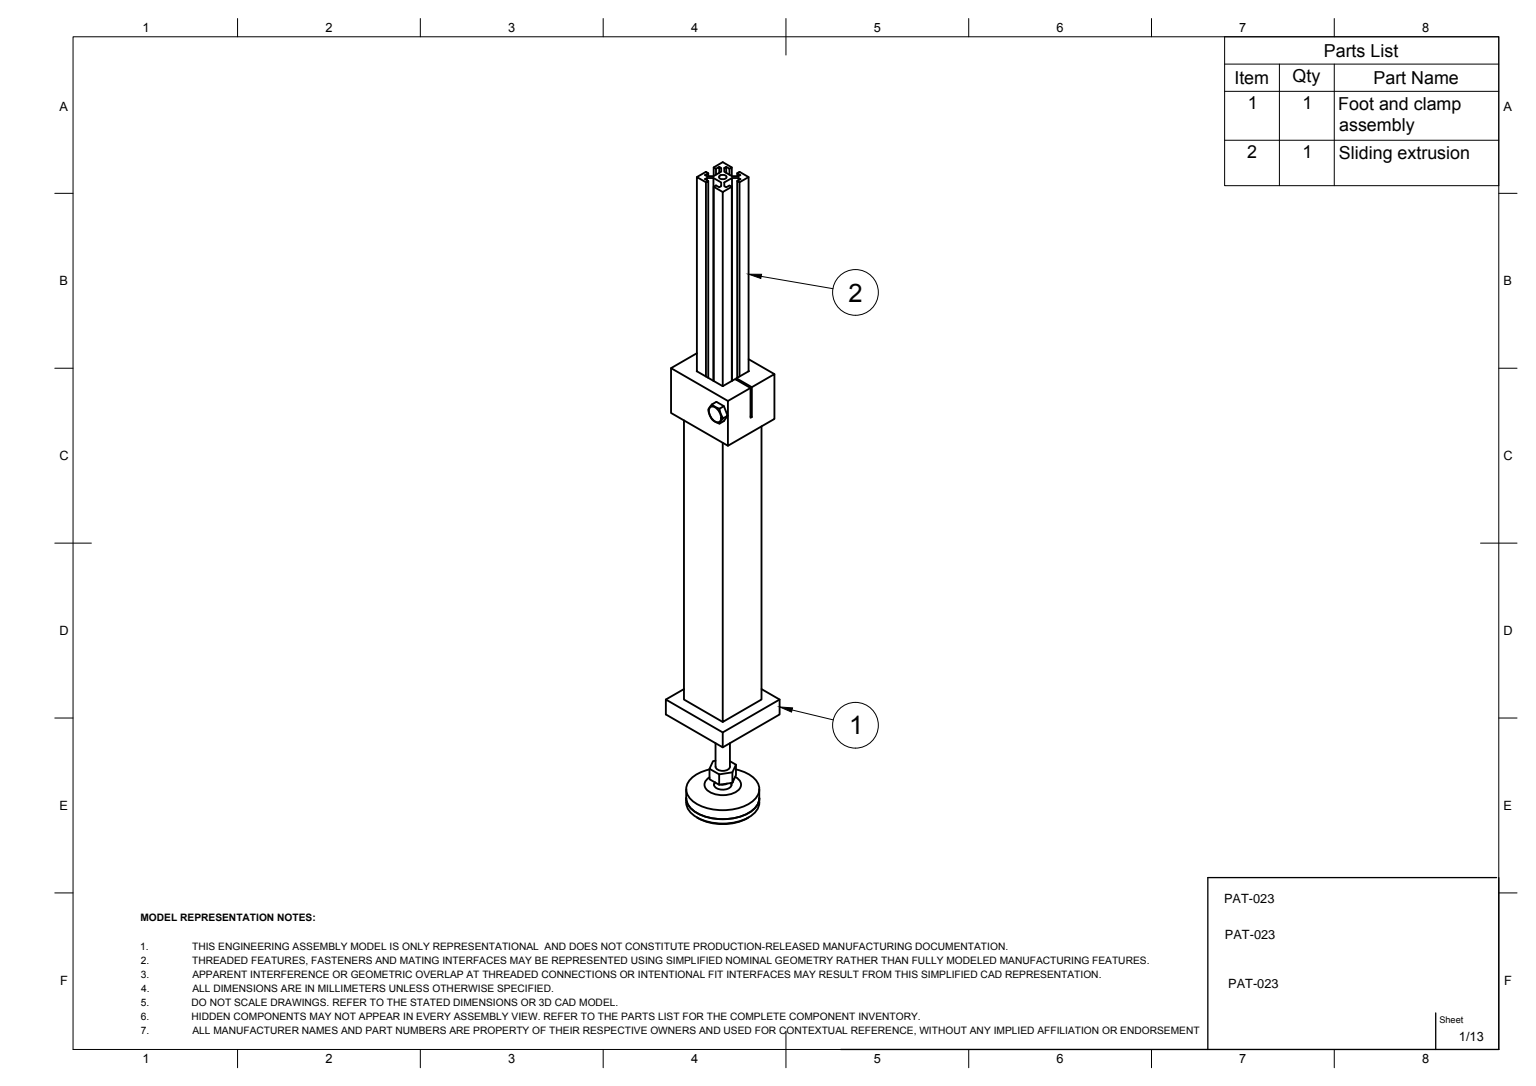
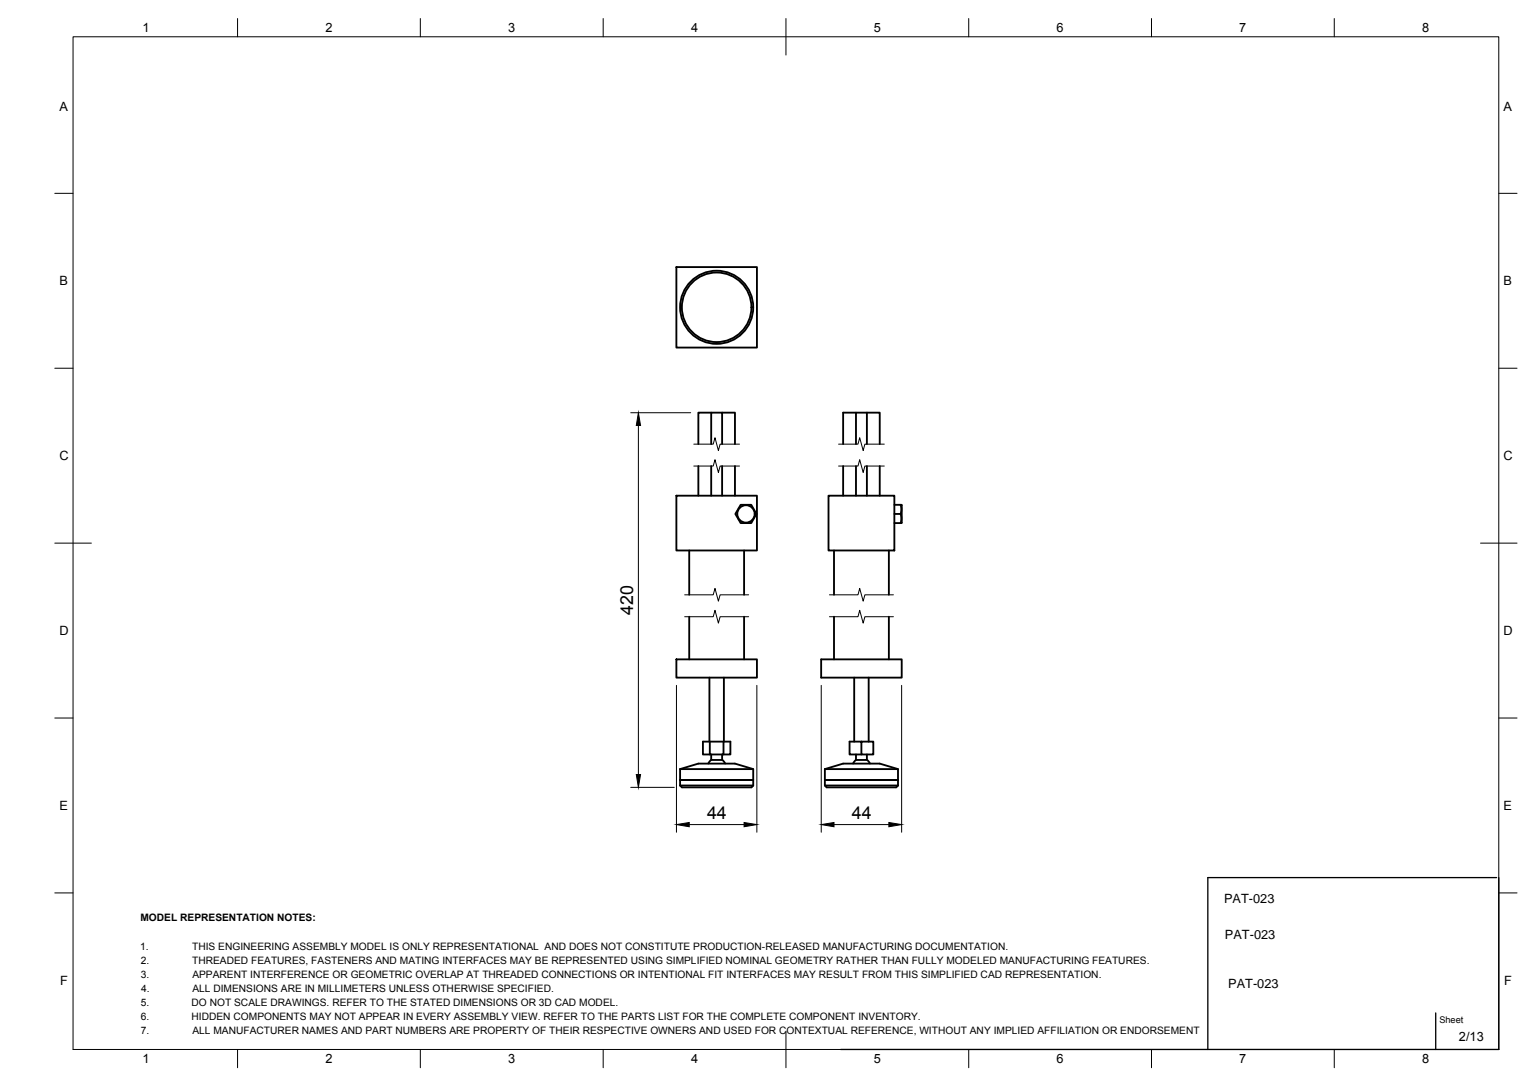
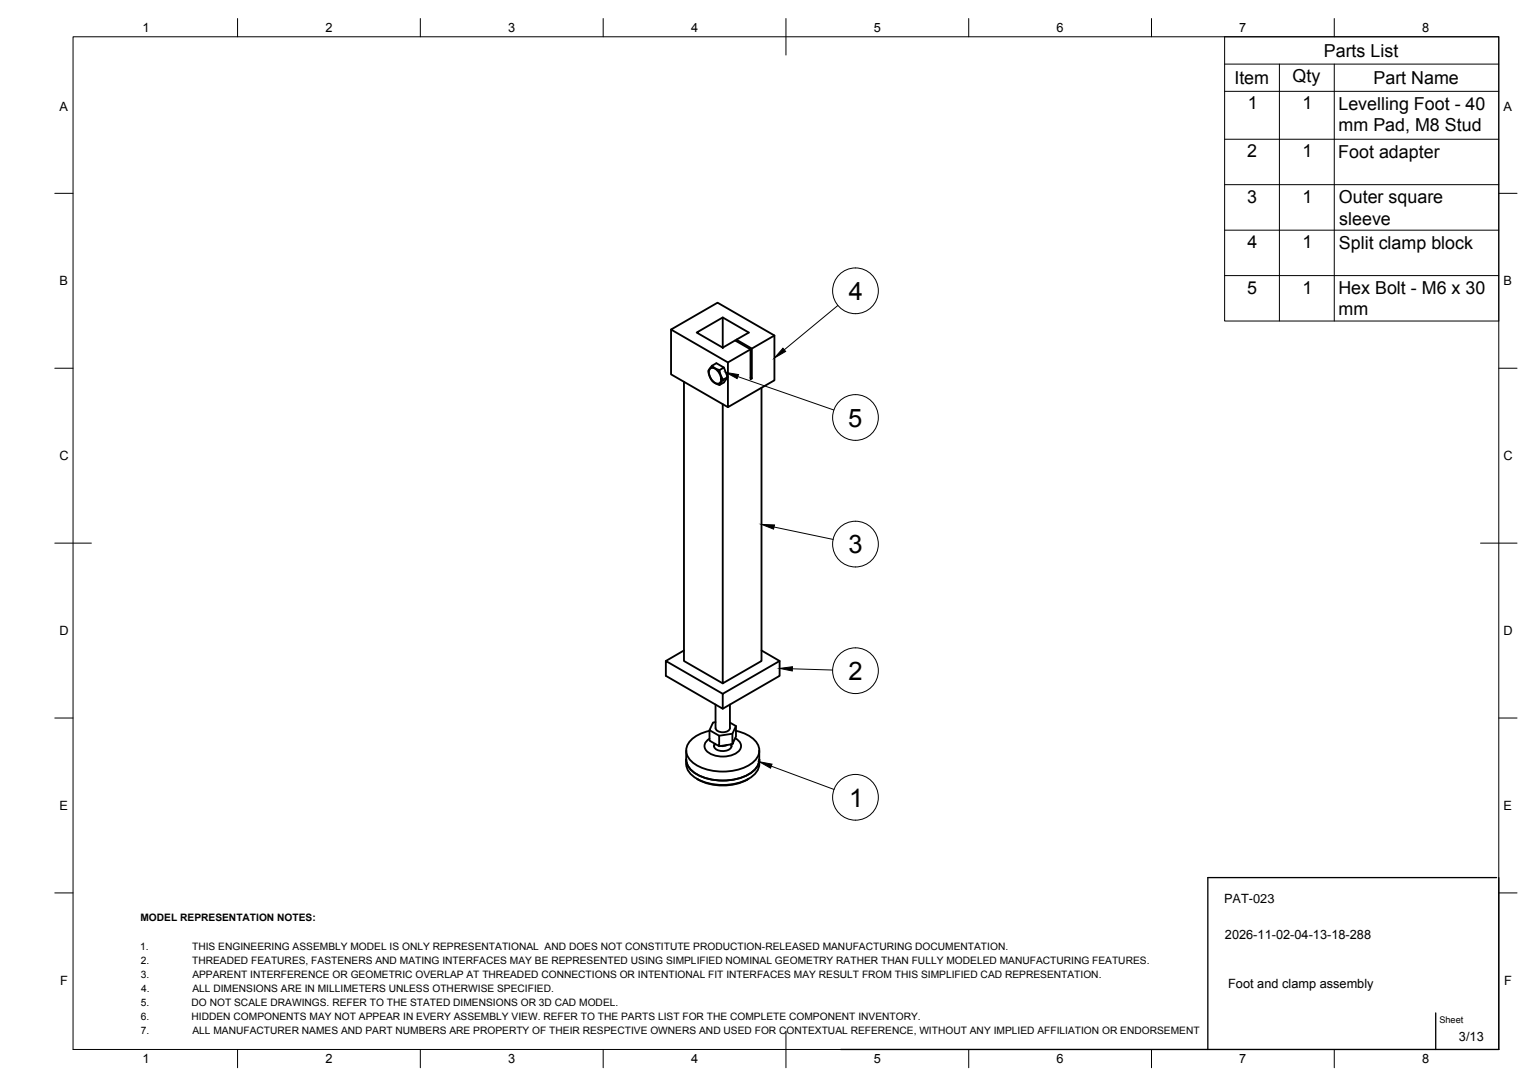
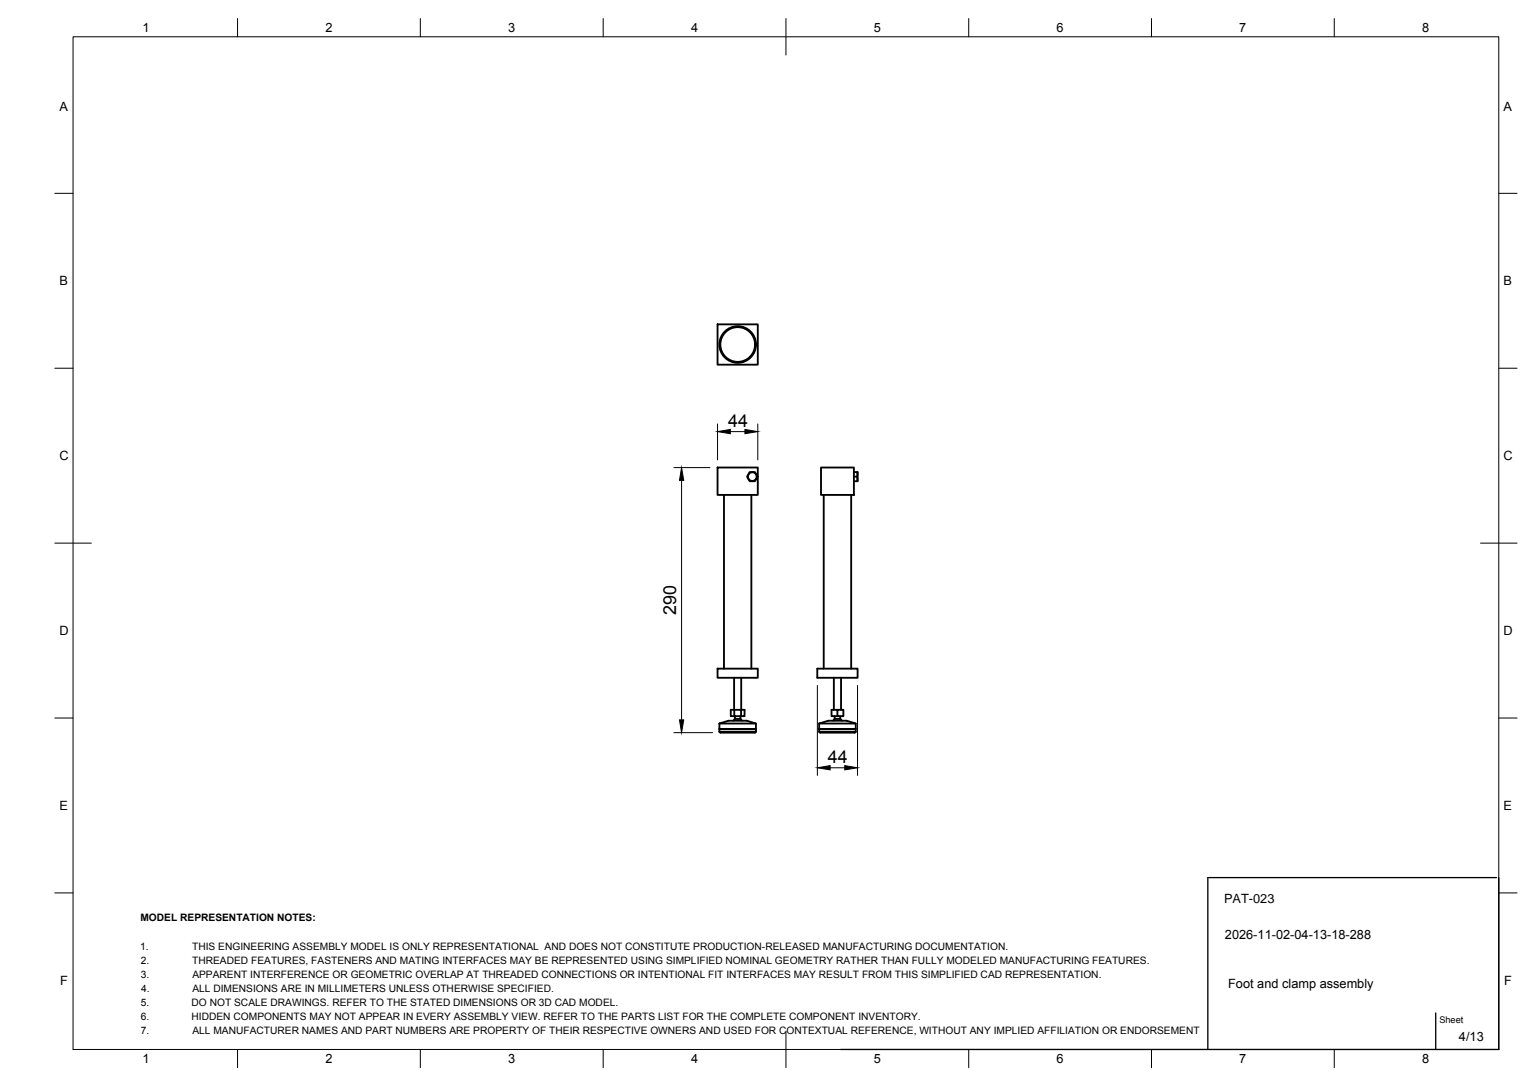
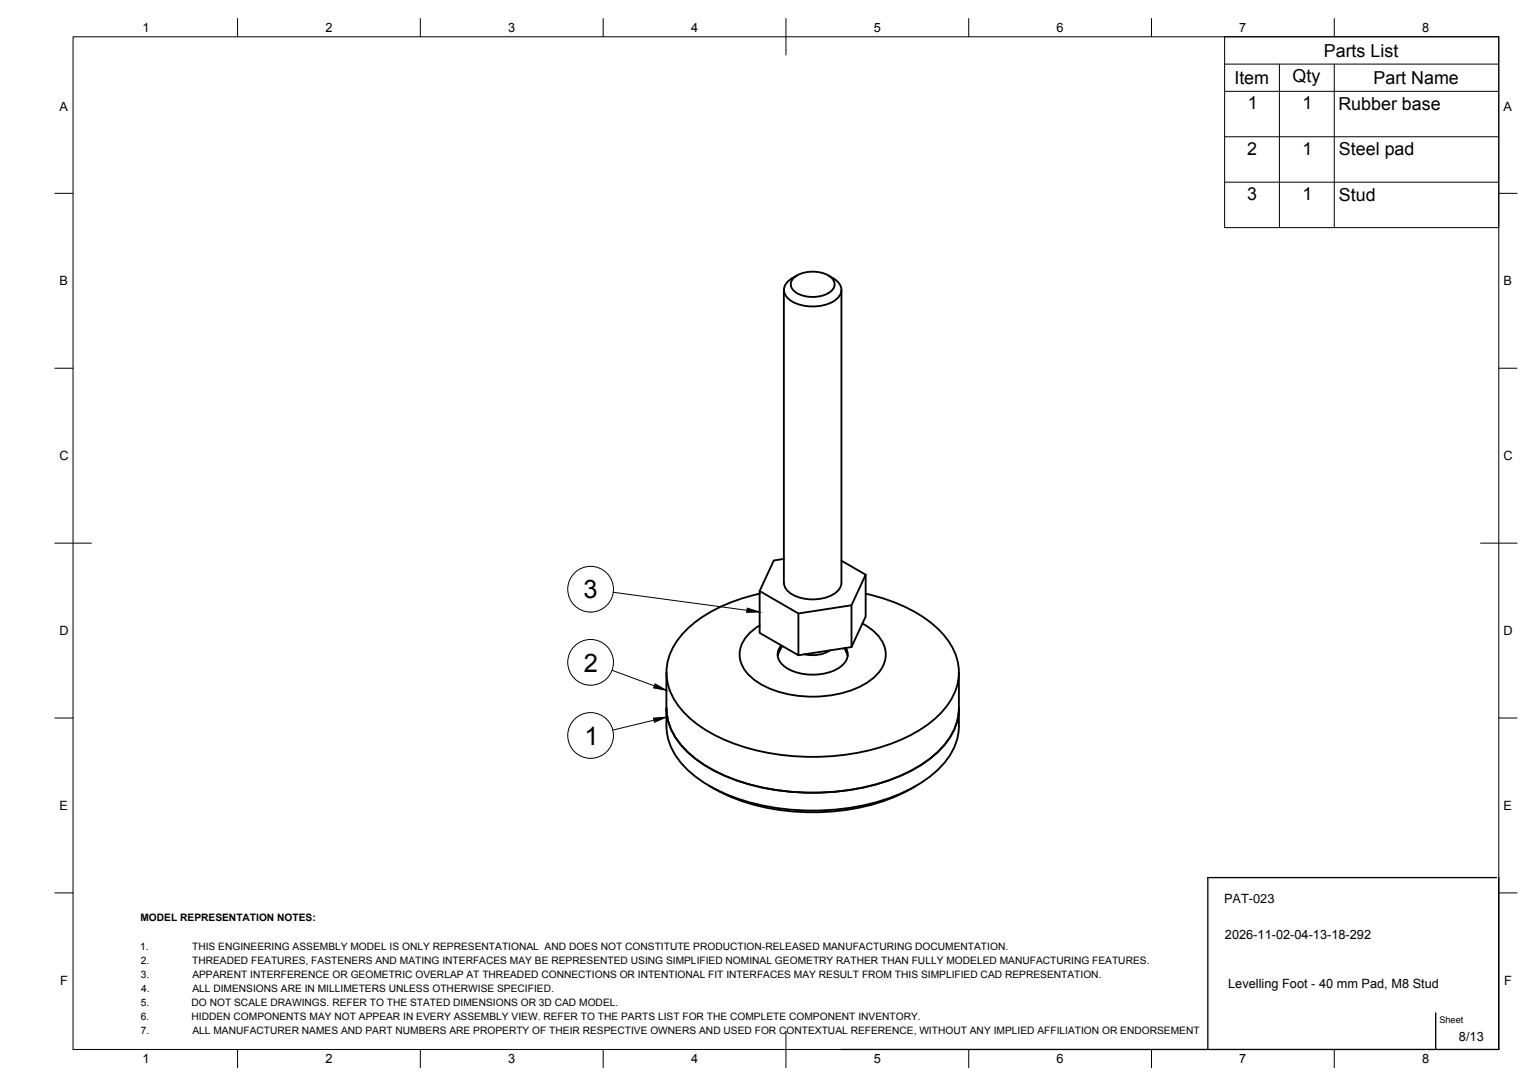
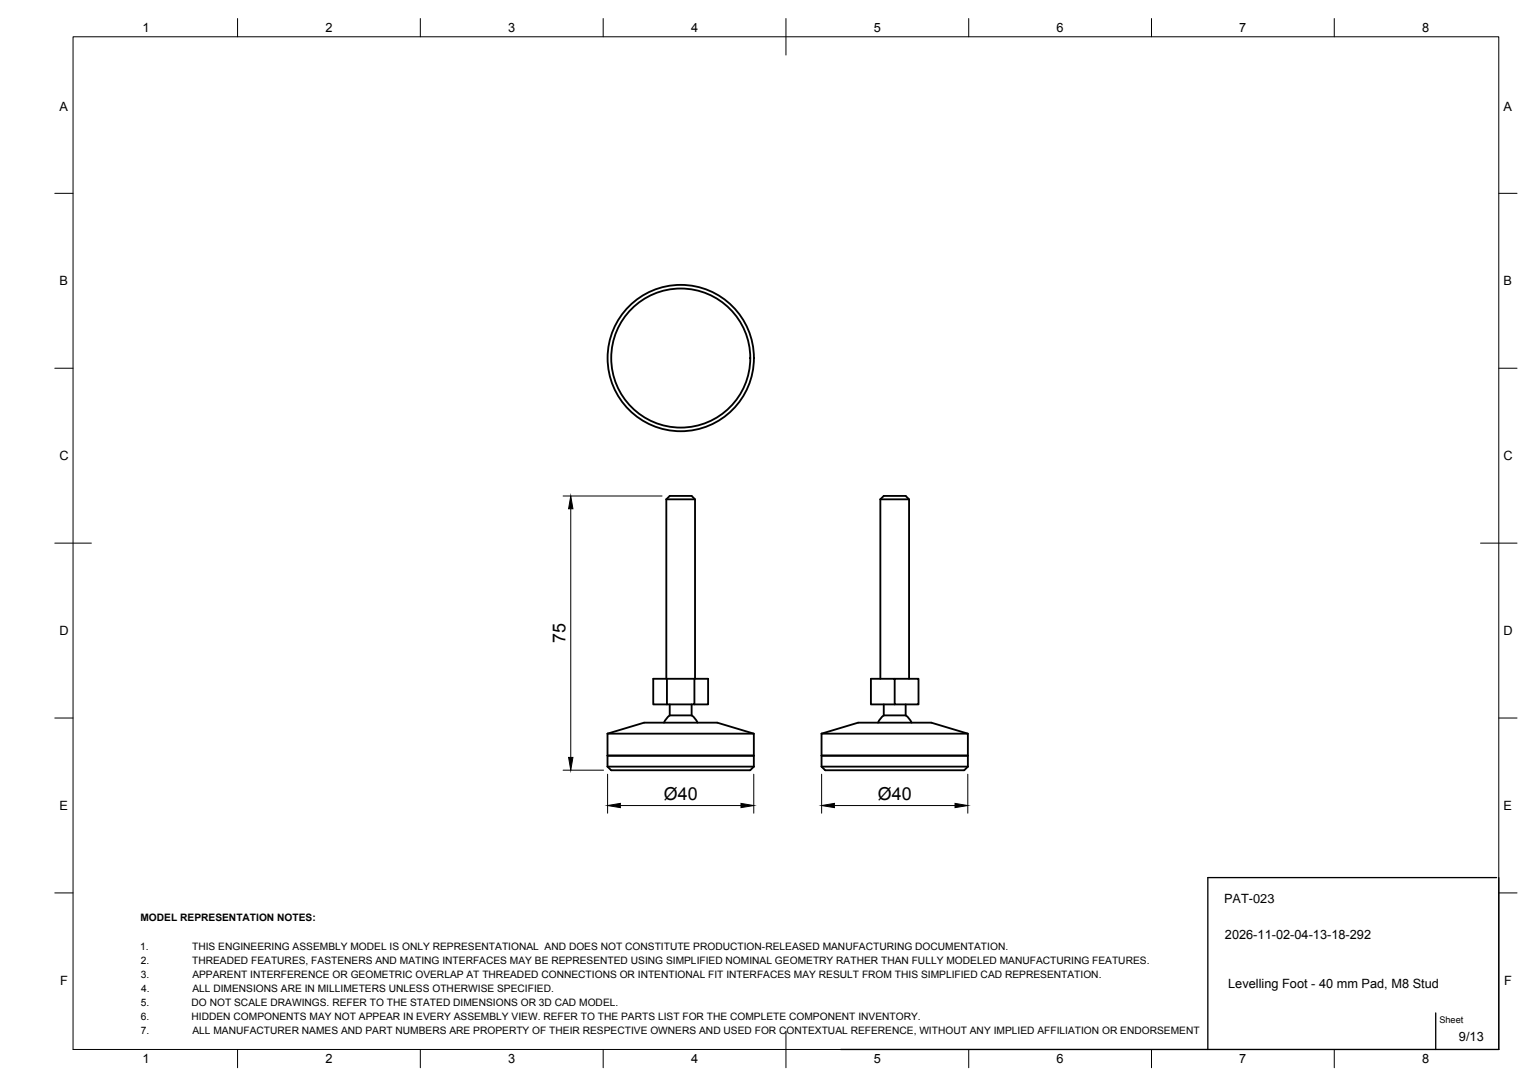
ISO-10303-21;
HEADER;
/* Generated by software containing ST-Developer
 * from STEP Tools, Inc. (www.steptools.com) 
 */

FILE_DESCRIPTION(
/* description */ ('PAT-023'),
/* implementation_level */ '2;1');

FILE_NAME(
/* name */ 'PAT-023',
/* time_stamp */ '2026-10-29T15:47:46-07:00',
/* author */ (''),
/* organization */ (''),
/* preprocessor_version */ 'ST-DEVELOPER v20.2',
/* originating_system */ 'Autodesk Translation Framework v15.17.0.0',
/* authorisation */ '');

FILE_SCHEMA (('AUTOMOTIVE_DESIGN { 1 0 10303 214 3 1 1 }'));
ENDSEC;

DATA;
#10=MECHANICAL_DESIGN_GEOMETRIC_PRESENTATION_REPRESENTATION('',(#84,#85,
#86,#87,#88,#89,#90,#91),#3773);
#11=(
BOUNDED_CURVE()
B_SPLINE_CURVE(2,(#3418,#3419,#3420),.UNSPECIFIED.,.F.,.F.)
B_SPLINE_CURVE_WITH_KNOTS((3,3),(0.144988513094728,0.791574906712449),
 .UNSPECIFIED.)
CURVE()
GEOMETRIC_REPRESENTATION_ITEM()
RATIONAL_B_SPLINE_CURVE((1.09282032302755,1.26188021535082,1.09282032302931))
REPRESENTATION_ITEM('')
);
#12=(
BOUNDED_CURVE()
B_SPLINE_CURVE(2,(#3422,#3423,#3424),.UNSPECIFIED.,.F.,.F.)
B_SPLINE_CURVE_WITH_KNOTS((3,3),(0.144988513094728,0.791574906712449),
 .UNSPECIFIED.)
CURVE()
GEOMETRIC_REPRESENTATION_ITEM()
RATIONAL_B_SPLINE_CURVE((1.09282032302755,1.26188021535082,1.09282032302931))
REPRESENTATION_ITEM('')
);
#13=(
BOUNDED_CURVE()
B_SPLINE_CURVE(2,(#3426,#3427,#3428),.UNSPECIFIED.,.F.,.F.)
B_SPLINE_CURVE_WITH_KNOTS((3,3),(0.144988513094728,0.791574906712449),
 .UNSPECIFIED.)
CURVE()
GEOMETRIC_REPRESENTATION_ITEM()
RATIONAL_B_SPLINE_CURVE((1.09282032302755,1.26188021535082,1.09282032302931))
REPRESENTATION_ITEM('')
);
#14=(
BOUNDED_CURVE()
B_SPLINE_CURVE(2,(#3430,#3431,#3432),.UNSPECIFIED.,.F.,.F.)
B_SPLINE_CURVE_WITH_KNOTS((3,3),(0.144988513094728,0.791574906712449),
 .UNSPECIFIED.)
CURVE()
GEOMETRIC_REPRESENTATION_ITEM()
RATIONAL_B_SPLINE_CURVE((1.09282032302755,1.26188021535082,1.09282032302931))
REPRESENTATION_ITEM('')
);
#15=(
BOUNDED_CURVE()
B_SPLINE_CURVE(2,(#3434,#3435,#3436),.UNSPECIFIED.,.F.,.F.)
B_SPLINE_CURVE_WITH_KNOTS((3,3),(0.144988513094728,0.791574906712449),
 .UNSPECIFIED.)
CURVE()
GEOMETRIC_REPRESENTATION_ITEM()
RATIONAL_B_SPLINE_CURVE((1.09282032302755,1.26188021535082,1.09282032302931))
REPRESENTATION_ITEM('')
);
#16=(
BOUNDED_CURVE()
B_SPLINE_CURVE(2,(#3437,#3438,#3439),.UNSPECIFIED.,.F.,.F.)
B_SPLINE_CURVE_WITH_KNOTS((3,3),(0.144988513094727,0.791574906712449),
 .UNSPECIFIED.)
CURVE()
GEOMETRIC_REPRESENTATION_ITEM()
RATIONAL_B_SPLINE_CURVE((1.09282032302755,1.26188021535082,1.09282032302931))
REPRESENTATION_ITEM('')
);
#17=ITEM_DEFINED_TRANSFORMATION($,$,#2384,#2423);
#18=ITEM_DEFINED_TRANSFORMATION($,$,#2392,#2424);
#19=ITEM_DEFINED_TRANSFORMATION($,$,#2403,#2425);
#20=ITEM_DEFINED_TRANSFORMATION($,$,#2336,#2443);
#21=ITEM_DEFINED_TRANSFORMATION($,$,#2346,#2444);
#22=ITEM_DEFINED_TRANSFORMATION($,$,#2357,#2445);
#23=ITEM_DEFINED_TRANSFORMATION($,$,#2383,#2446);
#24=ITEM_DEFINED_TRANSFORMATION($,$,#2426,#2447);
#25=ITEM_DEFINED_TRANSFORMATION($,$,#2449,#2499);
#26=ITEM_DEFINED_TRANSFORMATION($,$,#2335,#2500);
#27=ITEM_DEFINED_TRANSFORMATION($,$,#2448,#2501);
#28=(
REPRESENTATION_RELATIONSHIP($,$,#3819,#3818)
REPRESENTATION_RELATIONSHIP_WITH_TRANSFORMATION(#17)
SHAPE_REPRESENTATION_RELATIONSHIP()
);
#29=(
REPRESENTATION_RELATIONSHIP($,$,#3820,#3818)
REPRESENTATION_RELATIONSHIP_WITH_TRANSFORMATION(#18)
SHAPE_REPRESENTATION_RELATIONSHIP()
);
#30=(
REPRESENTATION_RELATIONSHIP($,$,#3821,#3818)
REPRESENTATION_RELATIONSHIP_WITH_TRANSFORMATION(#19)
SHAPE_REPRESENTATION_RELATIONSHIP()
);
#31=(
REPRESENTATION_RELATIONSHIP($,$,#3815,#3814)
REPRESENTATION_RELATIONSHIP_WITH_TRANSFORMATION(#20)
SHAPE_REPRESENTATION_RELATIONSHIP()
);
#32=(
REPRESENTATION_RELATIONSHIP($,$,#3816,#3814)
REPRESENTATION_RELATIONSHIP_WITH_TRANSFORMATION(#21)
SHAPE_REPRESENTATION_RELATIONSHIP()
);
#33=(
REPRESENTATION_RELATIONSHIP($,$,#3817,#3814)
REPRESENTATION_RELATIONSHIP_WITH_TRANSFORMATION(#22)
SHAPE_REPRESENTATION_RELATIONSHIP()
);
#34=(
REPRESENTATION_RELATIONSHIP($,$,#3818,#3814)
REPRESENTATION_RELATIONSHIP_WITH_TRANSFORMATION(#23)
SHAPE_REPRESENTATION_RELATIONSHIP()
);
#35=(
REPRESENTATION_RELATIONSHIP($,$,#3822,#3814)
REPRESENTATION_RELATIONSHIP_WITH_TRANSFORMATION(#24)
SHAPE_REPRESENTATION_RELATIONSHIP()
);
#36=(
REPRESENTATION_RELATIONSHIP($,$,#3824,#3823)
REPRESENTATION_RELATIONSHIP_WITH_TRANSFORMATION(#25)
SHAPE_REPRESENTATION_RELATIONSHIP()
);
#37=(
REPRESENTATION_RELATIONSHIP($,$,#3814,#3813)
REPRESENTATION_RELATIONSHIP_WITH_TRANSFORMATION(#26)
SHAPE_REPRESENTATION_RELATIONSHIP()
);
#38=(
REPRESENTATION_RELATIONSHIP($,$,#3823,#3813)
REPRESENTATION_RELATIONSHIP_WITH_TRANSFORMATION(#27)
SHAPE_REPRESENTATION_RELATIONSHIP()
);
#39=CONTEXT_DEPENDENT_SHAPE_REPRESENTATION(#28,#3799);
#40=CONTEXT_DEPENDENT_SHAPE_REPRESENTATION(#29,#3800);
#41=CONTEXT_DEPENDENT_SHAPE_REPRESENTATION(#30,#3801);
#42=CONTEXT_DEPENDENT_SHAPE_REPRESENTATION(#31,#3803);
#43=CONTEXT_DEPENDENT_SHAPE_REPRESENTATION(#32,#3804);
#44=CONTEXT_DEPENDENT_SHAPE_REPRESENTATION(#33,#3805);
#45=CONTEXT_DEPENDENT_SHAPE_REPRESENTATION(#34,#3806);
#46=CONTEXT_DEPENDENT_SHAPE_REPRESENTATION(#35,#3807);
#47=CONTEXT_DEPENDENT_SHAPE_REPRESENTATION(#36,#3810);
#48=CONTEXT_DEPENDENT_SHAPE_REPRESENTATION(#37,#3811);
#49=CONTEXT_DEPENDENT_SHAPE_REPRESENTATION(#38,#3812);
#50=NEXT_ASSEMBLY_USAGE_OCCURRENCE('Rubber base:1','Rubber base:1',
'Rubber base:1',#3831,#3832,'Rubber base:1');
#51=NEXT_ASSEMBLY_USAGE_OCCURRENCE('Steel pad:1','Steel pad:1',
'Steel pad:1',#3831,#3833,'Steel pad:1');
#52=NEXT_ASSEMBLY_USAGE_OCCURRENCE('Stud:1','Stud:1','Stud:1',#3831,#3834,
'Stud:1');
#53=NEXT_ASSEMBLY_USAGE_OCCURRENCE('Foot adapter:1','Foot adapter:1',
'Foot adapter:1',#3827,#3828,'Foot adapter:1');
#54=NEXT_ASSEMBLY_USAGE_OCCURRENCE('Outer square sleeve:1',
'Outer square sleeve:1','Outer square sleeve:1',#3827,#3829,
'Outer square sleeve:1');
#55=NEXT_ASSEMBLY_USAGE_OCCURRENCE('Split clamp block:1',
'Split clamp block:1','Split clamp block:1',#3827,#3830,
'Split clamp block:1');
#56=NEXT_ASSEMBLY_USAGE_OCCURRENCE(
'Levelling Foot - 40 mm Pad, M8 Stud:2',
'Levelling Foot - 40 mm Pad, M8 Stud:2',
'Levelling Foot - 40 mm Pad, M8 Stud:2',#3827,#3831,
'Levelling Foot - 40 mm Pad, M8 Stud:2');
#57=NEXT_ASSEMBLY_USAGE_OCCURRENCE('Hex Bolt - M6 x 30 mm:2',
'Hex Bolt - M6 x 30 mm:2','Hex Bolt - M6 x 30 mm:2',#3827,#3835,
'Hex Bolt - M6 x 30 mm:2');
#58=NEXT_ASSEMBLY_USAGE_OCCURRENCE(
'Slotted Extrusion - 20 x 20 x 300 mm:2',
'Slotted Extrusion - 20 x 20 x 300 mm:2',
'Slotted Extrusion - 20 x 20 x 300 mm:2',#3836,#3837,
'Slotted Extrusion - 20 x 20 x 300 mm:2');
#59=NEXT_ASSEMBLY_USAGE_OCCURRENCE('Foot and clamp assembly:1',
'Foot and clamp assembly:1','Foot and clamp assembly:1',#3826,#3827,
'Foot and clamp assembly:1');
#60=NEXT_ASSEMBLY_USAGE_OCCURRENCE('Sliding extrusion:1',
'Sliding extrusion:1','Sliding extrusion:1',#3826,#3836,
'Sliding extrusion:1');
#61=SPHERICAL_SURFACE('',#2393,0.52);
#62=SPHERICAL_SURFACE('',#2421,0.5);
#63=CONICAL_SURFACE('',#2387,1.95,0.785398163397449);
#64=CONICAL_SURFACE('',#2400,1.5,1.27933953231703);
#65=CONICAL_SURFACE('',#2418,0.35,0.78539816339745);
#66=CONICAL_SURFACE('',#2430,0.27,0.785398163397448);
#67=CONICAL_SURFACE('',#2433,0.576175134594813,1.0471975511966);
#68=SHAPE_REPRESENTATION_RELATIONSHIP('SRR','None',#3815,#76);
#69=SHAPE_REPRESENTATION_RELATIONSHIP('SRR','None',#3816,#77);
#70=SHAPE_REPRESENTATION_RELATIONSHIP('SRR','None',#3817,#78);
#71=SHAPE_REPRESENTATION_RELATIONSHIP('SRR','None',#3819,#79);
#72=SHAPE_REPRESENTATION_RELATIONSHIP('SRR','None',#3820,#80);
#73=SHAPE_REPRESENTATION_RELATIONSHIP('SRR','None',#3821,#81);
#74=SHAPE_REPRESENTATION_RELATIONSHIP('SRR','None',#3822,#82);
#75=SHAPE_REPRESENTATION_RELATIONSHIP('SRR','None',#3824,#83);
#76=ADVANCED_BREP_SHAPE_REPRESENTATION('',(#92),#3763);
#77=ADVANCED_BREP_SHAPE_REPRESENTATION('',(#93),#3764);
#78=ADVANCED_BREP_SHAPE_REPRESENTATION('',(#94),#3765);
#79=ADVANCED_BREP_SHAPE_REPRESENTATION('',(#95),#3767);
#80=ADVANCED_BREP_SHAPE_REPRESENTATION('',(#96),#3768);
#81=ADVANCED_BREP_SHAPE_REPRESENTATION('',(#97),#3769);
#82=ADVANCED_BREP_SHAPE_REPRESENTATION('',(#98),#3770);
#83=ADVANCED_BREP_SHAPE_REPRESENTATION('',(#99),#3772);
#84=STYLED_ITEM('',(#3960),#92);
#85=STYLED_ITEM('',(#3939),#93);
#86=STYLED_ITEM('',(#3925),#94);
#87=STYLED_ITEM('',(#3953),#95);
#88=STYLED_ITEM('',(#3932),#96);
#89=STYLED_ITEM('',(#3953),#97);
#90=STYLED_ITEM('',(#3953),#98);
#91=STYLED_ITEM('',(#3960),#99);
#92=MANIFOLD_SOLID_BREP('Body1',#2237);
#93=MANIFOLD_SOLID_BREP('Body1',#2238);
#94=MANIFOLD_SOLID_BREP('Body1',#2239);
#95=MANIFOLD_SOLID_BREP('Body1',#2240);
#96=MANIFOLD_SOLID_BREP('Body1',#2241);
#97=MANIFOLD_SOLID_BREP('Body1',#2242);
#98=MANIFOLD_SOLID_BREP('Body1',#2243);
#99=MANIFOLD_SOLID_BREP('Body1',#2244);
#100=FACE_BOUND('',#343,.T.);
#101=FACE_BOUND('',#345,.T.);
#102=FACE_BOUND('',#355,.T.);
#103=FACE_BOUND('',#357,.T.);
#104=FACE_BOUND('',#361,.T.);
#105=FACE_BOUND('',#363,.T.);
#106=FACE_BOUND('',#378,.T.);
#107=FACE_BOUND('',#380,.T.);
#108=FACE_BOUND('',#383,.T.);
#109=FACE_BOUND('',#393,.T.);
#110=FACE_BOUND('',#395,.T.);
#111=FACE_BOUND('',#404,.T.);
#112=FACE_BOUND('',#421,.T.);
#113=FACE_BOUND('',#468,.T.);
#114=FACE_BOUND('',#470,.T.);
#115=PLANE('',#2340);
#116=PLANE('',#2341);
#117=PLANE('',#2342);
#118=PLANE('',#2343);
#119=PLANE('',#2344);
#120=PLANE('',#2345);
#121=PLANE('',#2347);
#122=PLANE('',#2348);
#123=PLANE('',#2349);
#124=PLANE('',#2350);
#125=PLANE('',#2351);
#126=PLANE('',#2352);
#127=PLANE('',#2353);
#128=PLANE('',#2354);
#129=PLANE('',#2355);
#130=PLANE('',#2356);
#131=PLANE('',#2364);
#132=PLANE('',#2365);
#133=PLANE('',#2366);
#134=PLANE('',#2367);
#135=PLANE('',#2368);
#136=PLANE('',#2369);
#137=PLANE('',#2370);
#138=PLANE('',#2371);
#139=PLANE('',#2372);
#140=PLANE('',#2373);
#141=PLANE('',#2374);
#142=PLANE('',#2375);
#143=PLANE('',#2376);
#144=PLANE('',#2377);
#145=PLANE('',#2378);
#146=PLANE('',#2379);
#147=PLANE('',#2380);
#148=PLANE('',#2381);
#149=PLANE('',#2382);
#150=PLANE('',#2385);
#151=PLANE('',#2391);
#152=PLANE('',#2396);
#153=PLANE('',#2402);
#154=PLANE('',#2404);
#155=PLANE('',#2406);
#156=PLANE('',#2407);
#157=PLANE('',#2408);
#158=PLANE('',#2409);
#159=PLANE('',#2410);
#160=PLANE('',#2411);
#161=PLANE('',#2415);
#162=PLANE('',#2420);
#163=PLANE('',#2432);
#164=PLANE('',#2435);
#165=PLANE('',#2436);
#166=PLANE('',#2437);
#167=PLANE('',#2438);
#168=PLANE('',#2439);
#169=PLANE('',#2440);
#170=PLANE('',#2441);
#171=PLANE('',#2442);
#172=PLANE('',#2450);
#173=PLANE('',#2451);
#174=PLANE('',#2452);
#175=PLANE('',#2453);
#176=PLANE('',#2454);
#177=PLANE('',#2455);
#178=PLANE('',#2456);
#179=PLANE('',#2457);
#180=PLANE('',#2458);
#181=PLANE('',#2459);
#182=PLANE('',#2460);
#183=PLANE('',#2461);
#184=PLANE('',#2462);
#185=PLANE('',#2463);
#186=PLANE('',#2464);
#187=PLANE('',#2465);
#188=PLANE('',#2466);
#189=PLANE('',#2467);
#190=PLANE('',#2468);
#191=PLANE('',#2469);
#192=PLANE('',#2470);
#193=PLANE('',#2471);
#194=PLANE('',#2472);
#195=PLANE('',#2473);
#196=PLANE('',#2474);
#197=PLANE('',#2475);
#198=PLANE('',#2476);
#199=PLANE('',#2477);
#200=PLANE('',#2478);
#201=PLANE('',#2479);
#202=PLANE('',#2480);
#203=PLANE('',#2481);
#204=PLANE('',#2482);
#205=PLANE('',#2483);
#206=PLANE('',#2484);
#207=PLANE('',#2485);
#208=PLANE('',#2489);
#209=PLANE('',#2490);
#210=PLANE('',#2491);
#211=PLANE('',#2492);
#212=PLANE('',#2493);
#213=PLANE('',#2494);
#214=PLANE('',#2495);
#215=PLANE('',#2496);
#216=PLANE('',#2497);
#217=PLANE('',#2498);
#218=FACE_OUTER_BOUND('',#337,.T.);
#219=FACE_OUTER_BOUND('',#338,.T.);
#220=FACE_OUTER_BOUND('',#339,.T.);
#221=FACE_OUTER_BOUND('',#340,.T.);
#222=FACE_OUTER_BOUND('',#341,.T.);
#223=FACE_OUTER_BOUND('',#342,.T.);
#224=FACE_OUTER_BOUND('',#344,.T.);
#225=FACE_OUTER_BOUND('',#346,.T.);
#226=FACE_OUTER_BOUND('',#347,.T.);
#227=FACE_OUTER_BOUND('',#348,.T.);
#228=FACE_OUTER_BOUND('',#349,.T.);
#229=FACE_OUTER_BOUND('',#350,.T.);
#230=FACE_OUTER_BOUND('',#351,.T.);
#231=FACE_OUTER_BOUND('',#352,.T.);
#232=FACE_OUTER_BOUND('',#353,.T.);
#233=FACE_OUTER_BOUND('',#354,.T.);
#234=FACE_OUTER_BOUND('',#356,.T.);
#235=FACE_OUTER_BOUND('',#358,.T.);
#236=FACE_OUTER_BOUND('',#359,.T.);
#237=FACE_OUTER_BOUND('',#360,.T.);
#238=FACE_OUTER_BOUND('',#362,.T.);
#239=FACE_OUTER_BOUND('',#364,.T.);
#240=FACE_OUTER_BOUND('',#365,.T.);
#241=FACE_OUTER_BOUND('',#366,.T.);
#242=FACE_OUTER_BOUND('',#367,.T.);
#243=FACE_OUTER_BOUND('',#368,.T.);
#244=FACE_OUTER_BOUND('',#369,.T.);
#245=FACE_OUTER_BOUND('',#370,.T.);
#246=FACE_OUTER_BOUND('',#371,.T.);
#247=FACE_OUTER_BOUND('',#372,.T.);
#248=FACE_OUTER_BOUND('',#373,.T.);
#249=FACE_OUTER_BOUND('',#374,.T.);
#250=FACE_OUTER_BOUND('',#375,.T.);
#251=FACE_OUTER_BOUND('',#376,.T.);
#252=FACE_OUTER_BOUND('',#377,.T.);
#253=FACE_OUTER_BOUND('',#379,.T.);
#254=FACE_OUTER_BOUND('',#381,.T.);
#255=FACE_OUTER_BOUND('',#382,.T.);
#256=FACE_OUTER_BOUND('',#384,.T.);
#257=FACE_OUTER_BOUND('',#385,.T.);
#258=FACE_OUTER_BOUND('',#386,.T.);
#259=FACE_OUTER_BOUND('',#387,.T.);
#260=FACE_OUTER_BOUND('',#388,.T.);
#261=FACE_OUTER_BOUND('',#389,.T.);
#262=FACE_OUTER_BOUND('',#390,.T.);
#263=FACE_OUTER_BOUND('',#391,.T.);
#264=FACE_OUTER_BOUND('',#392,.T.);
#265=FACE_OUTER_BOUND('',#394,.T.);
#266=FACE_OUTER_BOUND('',#396,.T.);
#267=FACE_OUTER_BOUND('',#397,.T.);
#268=FACE_OUTER_BOUND('',#398,.T.);
#269=FACE_OUTER_BOUND('',#399,.T.);
#270=FACE_OUTER_BOUND('',#400,.T.);
#271=FACE_OUTER_BOUND('',#401,.T.);
#272=FACE_OUTER_BOUND('',#402,.T.);
#273=FACE_OUTER_BOUND('',#403,.T.);
#274=FACE_OUTER_BOUND('',#405,.T.);
#275=FACE_OUTER_BOUND('',#406,.T.);
#276=FACE_OUTER_BOUND('',#407,.T.);
#277=FACE_OUTER_BOUND('',#408,.T.);
#278=FACE_OUTER_BOUND('',#409,.T.);
#279=FACE_OUTER_BOUND('',#410,.T.);
#280=FACE_OUTER_BOUND('',#411,.T.);
#281=FACE_OUTER_BOUND('',#412,.T.);
#282=FACE_OUTER_BOUND('',#413,.T.);
#283=FACE_OUTER_BOUND('',#414,.T.);
#284=FACE_OUTER_BOUND('',#415,.T.);
#285=FACE_OUTER_BOUND('',#416,.T.);
#286=FACE_OUTER_BOUND('',#417,.T.);
#287=FACE_OUTER_BOUND('',#418,.T.);
#288=FACE_OUTER_BOUND('',#419,.T.);
#289=FACE_OUTER_BOUND('',#420,.T.);
#290=FACE_OUTER_BOUND('',#422,.T.);
#291=FACE_OUTER_BOUND('',#423,.T.);
#292=FACE_OUTER_BOUND('',#424,.T.);
#293=FACE_OUTER_BOUND('',#425,.T.);
#294=FACE_OUTER_BOUND('',#426,.T.);
#295=FACE_OUTER_BOUND('',#427,.T.);
#296=FACE_OUTER_BOUND('',#428,.T.);
#297=FACE_OUTER_BOUND('',#429,.T.);
#298=FACE_OUTER_BOUND('',#430,.T.);
#299=FACE_OUTER_BOUND('',#431,.T.);
#300=FACE_OUTER_BOUND('',#432,.T.);
#301=FACE_OUTER_BOUND('',#433,.T.);
#302=FACE_OUTER_BOUND('',#434,.T.);
#303=FACE_OUTER_BOUND('',#435,.T.);
#304=FACE_OUTER_BOUND('',#436,.T.);
#305=FACE_OUTER_BOUND('',#437,.T.);
#306=FACE_OUTER_BOUND('',#438,.T.);
#307=FACE_OUTER_BOUND('',#439,.T.);
#308=FACE_OUTER_BOUND('',#440,.T.);
#309=FACE_OUTER_BOUND('',#441,.T.);
#310=FACE_OUTER_BOUND('',#442,.T.);
#311=FACE_OUTER_BOUND('',#443,.T.);
#312=FACE_OUTER_BOUND('',#444,.T.);
#313=FACE_OUTER_BOUND('',#445,.T.);
#314=FACE_OUTER_BOUND('',#446,.T.);
#315=FACE_OUTER_BOUND('',#447,.T.);
#316=FACE_OUTER_BOUND('',#448,.T.);
#317=FACE_OUTER_BOUND('',#449,.T.);
#318=FACE_OUTER_BOUND('',#450,.T.);
#319=FACE_OUTER_BOUND('',#451,.T.);
#320=FACE_OUTER_BOUND('',#452,.T.);
#321=FACE_OUTER_BOUND('',#453,.T.);
#322=FACE_OUTER_BOUND('',#454,.T.);
#323=FACE_OUTER_BOUND('',#455,.T.);
#324=FACE_OUTER_BOUND('',#456,.T.);
#325=FACE_OUTER_BOUND('',#457,.T.);
#326=FACE_OUTER_BOUND('',#458,.T.);
#327=FACE_OUTER_BOUND('',#459,.T.);
#328=FACE_OUTER_BOUND('',#460,.T.);
#329=FACE_OUTER_BOUND('',#461,.T.);
#330=FACE_OUTER_BOUND('',#462,.T.);
#331=FACE_OUTER_BOUND('',#463,.T.);
#332=FACE_OUTER_BOUND('',#464,.T.);
#333=FACE_OUTER_BOUND('',#465,.T.);
#334=FACE_OUTER_BOUND('',#466,.T.);
#335=FACE_OUTER_BOUND('',#467,.T.);
#336=FACE_OUTER_BOUND('',#469,.T.);
#337=EDGE_LOOP('',(#1517,#1518,#1519,#1520));
#338=EDGE_LOOP('',(#1521,#1522,#1523,#1524));
#339=EDGE_LOOP('',(#1525,#1526,#1527,#1528));
#340=EDGE_LOOP('',(#1529,#1530,#1531,#1532));
#341=EDGE_LOOP('',(#1533,#1534,#1535,#1536));
#342=EDGE_LOOP('',(#1537,#1538,#1539,#1540));
#343=EDGE_LOOP('',(#1541));
#344=EDGE_LOOP('',(#1542,#1543,#1544,#1545));
#345=EDGE_LOOP('',(#1546));
#346=EDGE_LOOP('',(#1547,#1548,#1549,#1550));
#347=EDGE_LOOP('',(#1551,#1552,#1553,#1554));
#348=EDGE_LOOP('',(#1555,#1556,#1557,#1558));
#349=EDGE_LOOP('',(#1559,#1560,#1561,#1562));
#350=EDGE_LOOP('',(#1563,#1564,#1565,#1566));
#351=EDGE_LOOP('',(#1567,#1568,#1569,#1570));
#352=EDGE_LOOP('',(#1571,#1572,#1573,#1574));
#353=EDGE_LOOP('',(#1575,#1576,#1577,#1578));
#354=EDGE_LOOP('',(#1579,#1580,#1581,#1582));
#355=EDGE_LOOP('',(#1583,#1584,#1585,#1586));
#356=EDGE_LOOP('',(#1587,#1588,#1589,#1590));
#357=EDGE_LOOP('',(#1591,#1592,#1593,#1594));
#358=EDGE_LOOP('',(#1595,#1596,#1597,#1598));
#359=EDGE_LOOP('',(#1599,#1600,#1601,#1602));
#360=EDGE_LOOP('',(#1603,#1604,#1605,#1606,#1607));
#361=EDGE_LOOP('',(#1608));
#362=EDGE_LOOP('',(#1609,#1610,#1611,#1612,#1613));
#363=EDGE_LOOP('',(#1614));
#364=EDGE_LOOP('',(#1615,#1616,#1617,#1618));
#365=EDGE_LOOP('',(#1619,#1620,#1621,#1622,#1623,#1624,#1625,#1626,#1627,
#1628,#1629,#1630));
#366=EDGE_LOOP('',(#1631,#1632,#1633,#1634));
#367=EDGE_LOOP('',(#1635,#1636,#1637,#1638));
#368=EDGE_LOOP('',(#1639,#1640,#1641,#1642,#1643,#1644,#1645,#1646));
#369=EDGE_LOOP('',(#1647,#1648,#1649,#1650,#1651,#1652,#1653,#1654,#1655,
#1656,#1657,#1658));
#370=EDGE_LOOP('',(#1659,#1660,#1661,#1662));
#371=EDGE_LOOP('',(#1663,#1664,#1665,#1666));
#372=EDGE_LOOP('',(#1667,#1668,#1669,#1670));
#373=EDGE_LOOP('',(#1671,#1672,#1673,#1674));
#374=EDGE_LOOP('',(#1675,#1676,#1677,#1678,#1679,#1680));
#375=EDGE_LOOP('',(#1681,#1682,#1683,#1684));
#376=EDGE_LOOP('',(#1685,#1686,#1687,#1688));
#377=EDGE_LOOP('',(#1689,#1690,#1691,#1692));
#378=EDGE_LOOP('',(#1693));
#379=EDGE_LOOP('',(#1694,#1695,#1696,#1697));
#380=EDGE_LOOP('',(#1698));
#381=EDGE_LOOP('',(#1699,#1700,#1701,#1702));
#382=EDGE_LOOP('',(#1703,#1704,#1705,#1706));
#383=EDGE_LOOP('',(#1707,#1708,#1709,#1710));
#384=EDGE_LOOP('',(#1711));
#385=EDGE_LOOP('',(#1712,#1713,#1714,#1715));
#386=EDGE_LOOP('',(#1716,#1717,#1718,#1719));
#387=EDGE_LOOP('',(#1720));
#388=EDGE_LOOP('',(#1721,#1722,#1723));
#389=EDGE_LOOP('',(#1724));
#390=EDGE_LOOP('',(#1725,#1726,#1727,#1728));
#391=EDGE_LOOP('',(#1729,#1730,#1731,#1732));
#392=EDGE_LOOP('',(#1733));
#393=EDGE_LOOP('',(#1734));
#394=EDGE_LOOP('',(#1735,#1736,#1737,#1738,#1739,#1740));
#395=EDGE_LOOP('',(#1741));
#396=EDGE_LOOP('',(#1742,#1743,#1744,#1745));
#397=EDGE_LOOP('',(#1746,#1747,#1748,#1749));
#398=EDGE_LOOP('',(#1750,#1751,#1752,#1753));
#399=EDGE_LOOP('',(#1754,#1755,#1756,#1757));
#400=EDGE_LOOP('',(#1758,#1759,#1760,#1761));
#401=EDGE_LOOP('',(#1762,#1763,#1764,#1765));
#402=EDGE_LOOP('',(#1766,#1767,#1768,#1769));
#403=EDGE_LOOP('',(#1770,#1771,#1772,#1773,#1774,#1775));
#404=EDGE_LOOP('',(#1776));
#405=EDGE_LOOP('',(#1777,#1778,#1779,#1780));
#406=EDGE_LOOP('',(#1781,#1782,#1783,#1784));
#407=EDGE_LOOP('',(#1785));
#408=EDGE_LOOP('',(#1786,#1787,#1788));
#409=EDGE_LOOP('',(#1789,#1790,#1791,#1792));
#410=EDGE_LOOP('',(#1793,#1794,#1795,#1796));
#411=EDGE_LOOP('',(#1797));
#412=EDGE_LOOP('',(#1798,#1799,#1800,#1801,#1802,#1803,#1804,#1805,#1806));
#413=EDGE_LOOP('',(#1807,#1808,#1809,#1810));
#414=EDGE_LOOP('',(#1811,#1812,#1813,#1814));
#415=EDGE_LOOP('',(#1815,#1816,#1817,#1818));
#416=EDGE_LOOP('',(#1819,#1820,#1821,#1822));
#417=EDGE_LOOP('',(#1823,#1824,#1825,#1826));
#418=EDGE_LOOP('',(#1827,#1828,#1829,#1830));
#419=EDGE_LOOP('',(#1831));
#420=EDGE_LOOP('',(#1832,#1833,#1834,#1835,#1836,#1837));
#421=EDGE_LOOP('',(#1838));
#422=EDGE_LOOP('',(#1839,#1840,#1841,#1842));
#423=EDGE_LOOP('',(#1843,#1844,#1845,#1846));
#424=EDGE_LOOP('',(#1847,#1848,#1849,#1850));
#425=EDGE_LOOP('',(#1851,#1852,#1853,#1854));
#426=EDGE_LOOP('',(#1855,#1856,#1857,#1858));
#427=EDGE_LOOP('',(#1859,#1860,#1861,#1862));
#428=EDGE_LOOP('',(#1863,#1864,#1865,#1866));
#429=EDGE_LOOP('',(#1867,#1868,#1869,#1870));
#430=EDGE_LOOP('',(#1871,#1872,#1873,#1874));
#431=EDGE_LOOP('',(#1875,#1876,#1877,#1878));
#432=EDGE_LOOP('',(#1879,#1880,#1881,#1882));
#433=EDGE_LOOP('',(#1883,#1884,#1885,#1886));
#434=EDGE_LOOP('',(#1887,#1888,#1889,#1890));
#435=EDGE_LOOP('',(#1891,#1892,#1893,#1894));
#436=EDGE_LOOP('',(#1895,#1896,#1897,#1898));
#437=EDGE_LOOP('',(#1899,#1900,#1901,#1902));
#438=EDGE_LOOP('',(#1903,#1904,#1905,#1906));
#439=EDGE_LOOP('',(#1907,#1908,#1909,#1910));
#440=EDGE_LOOP('',(#1911,#1912,#1913,#1914));
#441=EDGE_LOOP('',(#1915,#1916,#1917,#1918));
#442=EDGE_LOOP('',(#1919,#1920,#1921,#1922));
#443=EDGE_LOOP('',(#1923,#1924,#1925,#1926));
#444=EDGE_LOOP('',(#1927,#1928,#1929,#1930));
#445=EDGE_LOOP('',(#1931,#1932,#1933,#1934));
#446=EDGE_LOOP('',(#1935,#1936,#1937,#1938));
#447=EDGE_LOOP('',(#1939,#1940,#1941,#1942));
#448=EDGE_LOOP('',(#1943,#1944,#1945,#1946));
#449=EDGE_LOOP('',(#1947,#1948,#1949,#1950));
#450=EDGE_LOOP('',(#1951,#1952,#1953,#1954));
#451=EDGE_LOOP('',(#1955,#1956,#1957,#1958));
#452=EDGE_LOOP('',(#1959,#1960,#1961,#1962));
#453=EDGE_LOOP('',(#1963,#1964,#1965,#1966));
#454=EDGE_LOOP('',(#1967,#1968,#1969,#1970));
#455=EDGE_LOOP('',(#1971,#1972,#1973,#1974));
#456=EDGE_LOOP('',(#1975,#1976,#1977,#1978));
#457=EDGE_LOOP('',(#1979,#1980,#1981,#1982));
#458=EDGE_LOOP('',(#1983,#1984,#1985,#1986));
#459=EDGE_LOOP('',(#1987,#1988,#1989,#1990));
#460=EDGE_LOOP('',(#1991,#1992,#1993,#1994));
#461=EDGE_LOOP('',(#1995,#1996,#1997,#1998));
#462=EDGE_LOOP('',(#1999,#2000,#2001,#2002));
#463=EDGE_LOOP('',(#2003,#2004,#2005,#2006));
#464=EDGE_LOOP('',(#2007,#2008,#2009,#2010));
#465=EDGE_LOOP('',(#2011,#2012,#2013,#2014));
#466=EDGE_LOOP('',(#2015,#2016,#2017,#2018));
#467=EDGE_LOOP('',(#2019,#2020,#2021,#2022,#2023,#2024,#2025,#2026,#2027,
#2028,#2029,#2030,#2031,#2032,#2033,#2034,#2035,#2036,#2037,#2038,#2039,
#2040,#2041,#2042,#2043,#2044,#2045,#2046,#2047,#2048,#2049,#2050,#2051,
#2052,#2053,#2054,#2055,#2056,#2057,#2058,#2059,#2060,#2061,#2062));
#468=EDGE_LOOP('',(#2063));
#469=EDGE_LOOP('',(#2064,#2065,#2066,#2067,#2068,#2069,#2070,#2071,#2072,
#2073,#2074,#2075,#2076,#2077,#2078,#2079,#2080,#2081,#2082,#2083,#2084,
#2085,#2086,#2087,#2088,#2089,#2090,#2091,#2092,#2093,#2094,#2095,#2096,
#2097,#2098,#2099,#2100,#2101,#2102,#2103,#2104,#2105,#2106,#2107));
#470=EDGE_LOOP('',(#2108));
#471=LINE('',#3109,#735);
#472=LINE('',#3114,#736);
#473=LINE('',#3116,#737);
#474=LINE('',#3118,#738);
#475=LINE('',#3119,#739);
#476=LINE('',#3122,#740);
#477=LINE('',#3124,#741);
#478=LINE('',#3125,#742);
#479=LINE('',#3128,#743);
#480=LINE('',#3130,#744);
#481=LINE('',#3131,#745);
#482=LINE('',#3133,#746);
#483=LINE('',#3134,#747);
#484=LINE('',#3141,#748);
#485=LINE('',#3143,#749);
#486=LINE('',#3145,#750);
#487=LINE('',#3146,#751);
#488=LINE('',#3149,#752);
#489=LINE('',#3151,#753);
#490=LINE('',#3152,#754);
#491=LINE('',#3155,#755);
#492=LINE('',#3157,#756);
#493=LINE('',#3158,#757);
#494=LINE('',#3160,#758);
#495=LINE('',#3161,#759);
#496=LINE('',#3165,#760);
#497=LINE('',#3167,#761);
#498=LINE('',#3169,#762);
#499=LINE('',#3170,#763);
#500=LINE('',#3173,#764);
#501=LINE('',#3175,#765);
#502=LINE('',#3176,#766);
#503=LINE('',#3179,#767);
#504=LINE('',#3181,#768);
#505=LINE('',#3182,#769);
#506=LINE('',#3184,#770);
#507=LINE('',#3185,#771);
#508=LINE('',#3193,#772);
#509=LINE('',#3199,#773);
#510=LINE('',#3204,#774);
#511=LINE('',#3206,#775);
#512=LINE('',#3208,#776);
#513=LINE('',#3210,#777);
#514=LINE('',#3211,#778);
#515=LINE('',#3215,#779);
#516=LINE('',#3217,#780);
#517=LINE('',#3219,#781);
#518=LINE('',#3221,#782);
#519=LINE('',#3222,#783);
#520=LINE('',#3224,#784);
#521=LINE('',#3225,#785);
#522=LINE('',#3228,#786);
#523=LINE('',#3230,#787);
#524=LINE('',#3232,#788);
#525=LINE('',#3234,#789);
#526=LINE('',#3235,#790);
#527=LINE('',#3237,#791);
#528=LINE('',#3239,#792);
#529=LINE('',#3241,#793);
#530=LINE('',#3243,#794);
#531=LINE('',#3244,#795);
#532=LINE('',#3247,#796);
#533=LINE('',#3248,#797);
#534=LINE('',#3251,#798);
#535=LINE('',#3252,#799);
#536=LINE('',#3255,#800);
#537=LINE('',#3257,#801);
#538=LINE('',#3259,#802);
#539=LINE('',#3261,#803);
#540=LINE('',#3262,#804);
#541=LINE('',#3265,#805);
#542=LINE('',#3267,#806);
#543=LINE('',#3268,#807);
#544=LINE('',#3270,#808);
#545=LINE('',#3272,#809);
#546=LINE('',#3273,#810);
#547=LINE('',#3275,#811);
#548=LINE('',#3277,#812);
#549=LINE('',#3282,#813);
#550=LINE('',#3283,#814);
#551=LINE('',#3284,#815);
#552=LINE('',#3287,#816);
#553=LINE('',#3288,#817);
#554=LINE('',#3291,#818);
#555=LINE('',#3292,#819);
#556=LINE('',#3294,#820);
#557=LINE('',#3297,#821);
#558=LINE('',#3298,#822);
#559=LINE('',#3301,#823);
#560=LINE('',#3302,#824);
#561=LINE('',#3304,#825);
#562=LINE('',#3314,#826);
#563=LINE('',#3318,#827);
#564=LINE('',#3332,#828);
#565=LINE('',#3336,#829);
#566=LINE('',#3342,#830);
#567=LINE('',#3344,#831);
#568=LINE('',#3346,#832);
#569=LINE('',#3348,#833);
#570=LINE('',#3350,#834);
#571=LINE('',#3351,#835);
#572=LINE('',#3357,#836);
#573=LINE('',#3358,#837);
#574=LINE('',#3359,#838);
#575=LINE('',#3362,#839);
#576=LINE('',#3363,#840);
#577=LINE('',#3366,#841);
#578=LINE('',#3367,#842);
#579=LINE('',#3370,#843);
#580=LINE('',#3371,#844);
#581=LINE('',#3374,#845);
#582=LINE('',#3375,#846);
#583=LINE('',#3377,#847);
#584=LINE('',#3382,#848);
#585=LINE('',#3388,#849);
#586=LINE('',#3392,#850);
#587=LINE('',#3405,#851);
#588=LINE('',#3410,#852);
#589=LINE('',#3416,#853);
#590=LINE('',#3442,#854);
#591=LINE('',#3444,#855);
#592=LINE('',#3445,#856);
#593=LINE('',#3448,#857);
#594=LINE('',#3449,#858);
#595=LINE('',#3452,#859);
#596=LINE('',#3453,#860);
#597=LINE('',#3456,#861);
#598=LINE('',#3457,#862);
#599=LINE('',#3460,#863);
#600=LINE('',#3461,#864);
#601=LINE('',#3463,#865);
#602=LINE('',#3476,#866);
#603=LINE('',#3478,#867);
#604=LINE('',#3480,#868);
#605=LINE('',#3481,#869);
#606=LINE('',#3484,#870);
#607=LINE('',#3486,#871);
#608=LINE('',#3487,#872);
#609=LINE('',#3490,#873);
#610=LINE('',#3492,#874);
#611=LINE('',#3493,#875);
#612=LINE('',#3496,#876);
#613=LINE('',#3498,#877);
#614=LINE('',#3499,#878);
#615=LINE('',#3502,#879);
#616=LINE('',#3504,#880);
#617=LINE('',#3505,#881);
#618=LINE('',#3508,#882);
#619=LINE('',#3510,#883);
#620=LINE('',#3511,#884);
#621=LINE('',#3514,#885);
#622=LINE('',#3516,#886);
#623=LINE('',#3517,#887);
#624=LINE('',#3520,#888);
#625=LINE('',#3522,#889);
#626=LINE('',#3523,#890);
#627=LINE('',#3526,#891);
#628=LINE('',#3528,#892);
#629=LINE('',#3529,#893);
#630=LINE('',#3533,#894);
#631=LINE('',#3535,#895);
#632=LINE('',#3537,#896);
#633=LINE('',#3538,#897);
#634=LINE('',#3541,#898);
#635=LINE('',#3543,#899);
#636=LINE('',#3544,#900);
#637=LINE('',#3547,#901);
#638=LINE('',#3549,#902);
#639=LINE('',#3550,#903);
#640=LINE('',#3553,#904);
#641=LINE('',#3555,#905);
#642=LINE('',#3556,#906);
#643=LINE('',#3559,#907);
#644=LINE('',#3561,#908);
#645=LINE('',#3562,#909);
#646=LINE('',#3565,#910);
#647=LINE('',#3567,#911);
#648=LINE('',#3568,#912);
#649=LINE('',#3571,#913);
#650=LINE('',#3573,#914);
#651=LINE('',#3574,#915);
#652=LINE('',#3577,#916);
#653=LINE('',#3579,#917);
#654=LINE('',#3580,#918);
#655=LINE('',#3583,#919);
#656=LINE('',#3585,#920);
#657=LINE('',#3586,#921);
#658=LINE('',#3590,#922);
#659=LINE('',#3592,#923);
#660=LINE('',#3594,#924);
#661=LINE('',#3595,#925);
#662=LINE('',#3598,#926);
#663=LINE('',#3600,#927);
#664=LINE('',#3601,#928);
#665=LINE('',#3604,#929);
#666=LINE('',#3606,#930);
#667=LINE('',#3607,#931);
#668=LINE('',#3610,#932);
#669=LINE('',#3612,#933);
#670=LINE('',#3613,#934);
#671=LINE('',#3616,#935);
#672=LINE('',#3618,#936);
#673=LINE('',#3619,#937);
#674=LINE('',#3622,#938);
#675=LINE('',#3624,#939);
#676=LINE('',#3625,#940);
#677=LINE('',#3628,#941);
#678=LINE('',#3630,#942);
#679=LINE('',#3631,#943);
#680=LINE('',#3634,#944);
#681=LINE('',#3636,#945);
#682=LINE('',#3637,#946);
#683=LINE('',#3640,#947);
#684=LINE('',#3642,#948);
#685=LINE('',#3643,#949);
#686=LINE('',#3647,#950);
#687=LINE('',#3649,#951);
#688=LINE('',#3651,#952);
#689=LINE('',#3652,#953);
#690=LINE('',#3655,#954);
#691=LINE('',#3657,#955);
#692=LINE('',#3658,#956);
#693=LINE('',#3661,#957);
#694=LINE('',#3663,#958);
#695=LINE('',#3664,#959);
#696=LINE('',#3667,#960);
#697=LINE('',#3669,#961);
#698=LINE('',#3670,#962);
#699=LINE('',#3673,#963);
#700=LINE('',#3675,#964);
#701=LINE('',#3676,#965);
#702=LINE('',#3679,#966);
#703=LINE('',#3681,#967);
#704=LINE('',#3682,#968);
#705=LINE('',#3685,#969);
#706=LINE('',#3687,#970);
#707=LINE('',#3688,#971);
#708=LINE('',#3691,#972);
#709=LINE('',#3693,#973);
#710=LINE('',#3694,#974);
#711=LINE('',#3697,#975);
#712=LINE('',#3699,#976);
#713=LINE('',#3700,#977);
#714=LINE('',#3705,#978);
#715=LINE('',#3709,#979);
#716=LINE('',#3711,#980);
#717=LINE('',#3712,#981);
#718=LINE('',#3715,#982);
#719=LINE('',#3717,#983);
#720=LINE('',#3718,#984);
#721=LINE('',#3720,#985);
#722=LINE('',#3721,#986);
#723=LINE('',#3724,#987);
#724=LINE('',#3726,#988);
#725=LINE('',#3727,#989);
#726=LINE('',#3729,#990);
#727=LINE('',#3730,#991);
#728=LINE('',#3733,#992);
#729=LINE('',#3735,#993);
#730=LINE('',#3736,#994);
#731=LINE('',#3738,#995);
#732=LINE('',#3739,#996);
#733=LINE('',#3741,#997);
#734=LINE('',#3742,#998);
#735=VECTOR('',#2512,0.34);
#736=VECTOR('',#2517,1.);
#737=VECTOR('',#2518,1.);
#738=VECTOR('',#2519,1.);
#739=VECTOR('',#2520,1.);
#740=VECTOR('',#2523,1.);
#741=VECTOR('',#2524,1.);
#742=VECTOR('',#2525,1.);
#743=VECTOR('',#2528,1.);
#744=VECTOR('',#2529,1.);
#745=VECTOR('',#2530,1.);
#746=VECTOR('',#2533,1.);
#747=VECTOR('',#2534,1.);
#748=VECTOR('',#2543,1.);
#749=VECTOR('',#2544,1.);
#750=VECTOR('',#2545,1.);
#751=VECTOR('',#2546,1.);
#752=VECTOR('',#2549,1.);
#753=VECTOR('',#2550,1.);
#754=VECTOR('',#2551,1.);
#755=VECTOR('',#2554,1.);
#756=VECTOR('',#2555,1.);
#757=VECTOR('',#2556,1.);
#758=VECTOR('',#2559,1.);
#759=VECTOR('',#2560,1.);
#760=VECTOR('',#2563,1.);
#761=VECTOR('',#2564,1.);
#762=VECTOR('',#2565,1.);
#763=VECTOR('',#2566,1.);
#764=VECTOR('',#2569,1.);
#765=VECTOR('',#2570,1.);
#766=VECTOR('',#2571,1.);
#767=VECTOR('',#2574,1.);
#768=VECTOR('',#2575,1.);
#769=VECTOR('',#2576,1.);
#770=VECTOR('',#2579,1.);
#771=VECTOR('',#2580,1.);
#772=VECTOR('',#2591,0.25);
#773=VECTOR('',#2598,0.33);
#774=VECTOR('',#2603,1.);
#775=VECTOR('',#2604,1.);
#776=VECTOR('',#2605,1.);
#777=VECTOR('',#2606,1.);
#778=VECTOR('',#2607,1.);
#779=VECTOR('',#2610,1.);
#780=VECTOR('',#2611,1.);
#781=VECTOR('',#2612,1.);
#782=VECTOR('',#2613,1.);
#783=VECTOR('',#2614,1.);
#784=VECTOR('',#2617,1.);
#785=VECTOR('',#2618,1.);
#786=VECTOR('',#2621,1.);
#787=VECTOR('',#2622,1.);
#788=VECTOR('',#2623,1.);
#789=VECTOR('',#2624,1.);
#790=VECTOR('',#2625,1.);
#791=VECTOR('',#2626,1.);
#792=VECTOR('',#2627,1.);
#793=VECTOR('',#2628,1.);
#794=VECTOR('',#2629,1.);
#795=VECTOR('',#2630,1.);
#796=VECTOR('',#2633,1.);
#797=VECTOR('',#2634,1.);
#798=VECTOR('',#2637,1.);
#799=VECTOR('',#2638,1.);
#800=VECTOR('',#2641,1.);
#801=VECTOR('',#2642,1.);
#802=VECTOR('',#2643,1.);
#803=VECTOR('',#2644,1.);
#804=VECTOR('',#2645,1.);
#805=VECTOR('',#2648,1.);
#806=VECTOR('',#2649,1.);
#807=VECTOR('',#2650,1.);
#808=VECTOR('',#2651,1.);
#809=VECTOR('',#2652,1.);
#810=VECTOR('',#2653,1.);
#811=VECTOR('',#2656,1.);
#812=VECTOR('',#2659,1.);
#813=VECTOR('',#2664,1.);
#814=VECTOR('',#2665,1.);
#815=VECTOR('',#2666,1.);
#816=VECTOR('',#2669,1.);
#817=VECTOR('',#2670,1.);
#818=VECTOR('',#2673,1.);
#819=VECTOR('',#2674,1.);
#820=VECTOR('',#2677,1.);
#821=VECTOR('',#2680,1.);
#822=VECTOR('',#2681,1.);
#823=VECTOR('',#2684,1.);
#824=VECTOR('',#2685,1.);
#825=VECTOR('',#2688,1.);
#826=VECTOR('',#2703,1.95);
#827=VECTOR('',#2708,2.);
#828=VECTOR('',#2727,2.);
#829=VECTOR('',#2732,1.5);
#830=VECTOR('',#2739,1.);
#831=VECTOR('',#2740,1.);
#832=VECTOR('',#2741,1.);
#833=VECTOR('',#2742,1.);
#834=VECTOR('',#2743,1.);
#835=VECTOR('',#2744,1.);
#836=VECTOR('',#2749,1.);
#837=VECTOR('',#2750,1.);
#838=VECTOR('',#2751,1.);
#839=VECTOR('',#2754,1.);
#840=VECTOR('',#2755,1.);
#841=VECTOR('',#2758,1.);
#842=VECTOR('',#2759,1.);
#843=VECTOR('',#2762,1.);
#844=VECTOR('',#2763,1.);
#845=VECTOR('',#2766,1.);
#846=VECTOR('',#2767,1.);
#847=VECTOR('',#2770,1.);
#848=VECTOR('',#2775,0.3);
#849=VECTOR('',#2784,0.4);
#850=VECTOR('',#2789,0.35);
#851=VECTOR('',#2808,0.3);
#852=VECTOR('',#2815,0.27);
#853=VECTOR('',#2822,0.576175134594813);
#854=VECTOR('',#2825,1.);
#855=VECTOR('',#2826,1.);
#856=VECTOR('',#2827,1.);
#857=VECTOR('',#2830,1.);
#858=VECTOR('',#2831,1.);
#859=VECTOR('',#2834,1.);
#860=VECTOR('',#2835,1.);
#861=VECTOR('',#2838,1.);
#862=VECTOR('',#2839,1.);
#863=VECTOR('',#2842,1.);
#864=VECTOR('',#2843,1.);
#865=VECTOR('',#2846,1.);
#866=VECTOR('',#2867,1.);
#867=VECTOR('',#2868,1.);
#868=VECTOR('',#2869,1.);
#869=VECTOR('',#2870,1.);
#870=VECTOR('',#2873,1.);
#871=VECTOR('',#2874,1.);
#872=VECTOR('',#2875,1.);
#873=VECTOR('',#2878,1.);
#874=VECTOR('',#2879,1.);
#875=VECTOR('',#2880,1.);
#876=VECTOR('',#2883,1.);
#877=VECTOR('',#2884,1.);
#878=VECTOR('',#2885,1.);
#879=VECTOR('',#2888,1.);
#880=VECTOR('',#2889,1.);
#881=VECTOR('',#2890,1.);
#882=VECTOR('',#2893,1.);
#883=VECTOR('',#2894,1.);
#884=VECTOR('',#2895,1.);
#885=VECTOR('',#2898,1.);
#886=VECTOR('',#2899,1.);
#887=VECTOR('',#2900,1.);
#888=VECTOR('',#2903,1.);
#889=VECTOR('',#2904,1.);
#890=VECTOR('',#2905,1.);
#891=VECTOR('',#2908,1.);
#892=VECTOR('',#2909,1.);
#893=VECTOR('',#2910,1.);
#894=VECTOR('',#2913,1.);
#895=VECTOR('',#2914,1.);
#896=VECTOR('',#2915,1.);
#897=VECTOR('',#2916,1.);
#898=VECTOR('',#2919,1.);
#899=VECTOR('',#2920,1.);
#900=VECTOR('',#2921,1.);
#901=VECTOR('',#2924,1.);
#902=VECTOR('',#2925,1.);
#903=VECTOR('',#2926,1.);
#904=VECTOR('',#2929,1.);
#905=VECTOR('',#2930,1.);
#906=VECTOR('',#2931,1.);
#907=VECTOR('',#2934,1.);
#908=VECTOR('',#2935,1.);
#909=VECTOR('',#2936,1.);
#910=VECTOR('',#2939,1.);
#911=VECTOR('',#2940,1.);
#912=VECTOR('',#2941,1.);
#913=VECTOR('',#2944,1.);
#914=VECTOR('',#2945,1.);
#915=VECTOR('',#2946,1.);
#916=VECTOR('',#2949,1.);
#917=VECTOR('',#2950,1.);
#918=VECTOR('',#2951,1.);
#919=VECTOR('',#2954,1.);
#920=VECTOR('',#2955,1.);
#921=VECTOR('',#2956,1.);
#922=VECTOR('',#2959,1.);
#923=VECTOR('',#2960,1.);
#924=VECTOR('',#2961,1.);
#925=VECTOR('',#2962,1.);
#926=VECTOR('',#2965,1.);
#927=VECTOR('',#2966,1.);
#928=VECTOR('',#2967,1.);
#929=VECTOR('',#2970,1.);
#930=VECTOR('',#2971,1.);
#931=VECTOR('',#2972,1.);
#932=VECTOR('',#2975,1.);
#933=VECTOR('',#2976,1.);
#934=VECTOR('',#2977,1.);
#935=VECTOR('',#2980,1.);
#936=VECTOR('',#2981,1.);
#937=VECTOR('',#2982,1.);
#938=VECTOR('',#2985,1.);
#939=VECTOR('',#2986,1.);
#940=VECTOR('',#2987,1.);
#941=VECTOR('',#2990,1.);
#942=VECTOR('',#2991,1.);
#943=VECTOR('',#2992,1.);
#944=VECTOR('',#2995,1.);
#945=VECTOR('',#2996,1.);
#946=VECTOR('',#2997,1.);
#947=VECTOR('',#3000,1.);
#948=VECTOR('',#3001,1.);
#949=VECTOR('',#3002,1.);
#950=VECTOR('',#3005,1.);
#951=VECTOR('',#3006,1.);
#952=VECTOR('',#3007,1.);
#953=VECTOR('',#3008,1.);
#954=VECTOR('',#3011,1.);
#955=VECTOR('',#3012,1.);
#956=VECTOR('',#3013,1.);
#957=VECTOR('',#3016,1.);
#958=VECTOR('',#3017,1.);
#959=VECTOR('',#3018,1.);
#960=VECTOR('',#3021,1.);
#961=VECTOR('',#3022,1.);
#962=VECTOR('',#3023,1.);
#963=VECTOR('',#3026,1.);
#964=VECTOR('',#3027,1.);
#965=VECTOR('',#3028,1.);
#966=VECTOR('',#3031,1.);
#967=VECTOR('',#3032,1.);
#968=VECTOR('',#3033,1.);
#969=VECTOR('',#3036,1.);
#970=VECTOR('',#3037,1.);
#971=VECTOR('',#3038,1.);
#972=VECTOR('',#3041,1.);
#973=VECTOR('',#3042,1.);
#974=VECTOR('',#3043,1.);
#975=VECTOR('',#3046,1.);
#976=VECTOR('',#3047,1.);
#977=VECTOR('',#3048,1.);
#978=VECTOR('',#3053,0.21);
#979=VECTOR('',#3058,1.);
#980=VECTOR('',#3059,1.);
#981=VECTOR('',#3060,1.);
#982=VECTOR('',#3063,1.);
#983=VECTOR('',#3064,1.);
#984=VECTOR('',#3065,1.);
#985=VECTOR('',#3068,1.);
#986=VECTOR('',#3069,1.);
#987=VECTOR('',#3072,1.);
#988=VECTOR('',#3073,1.);
#989=VECTOR('',#3074,1.);
#990=VECTOR('',#3077,1.);
#991=VECTOR('',#3078,1.);
#992=VECTOR('',#3081,1.);
#993=VECTOR('',#3082,1.);
#994=VECTOR('',#3083,1.);
#995=VECTOR('',#3086,1.);
#996=VECTOR('',#3087,1.);
#997=VECTOR('',#3090,1.);
#998=VECTOR('',#3091,1.);
#999=CIRCLE('',#2338,0.34);
#1000=CIRCLE('',#2339,0.34);
#1001=CIRCLE('',#2359,0.25);
#1002=CIRCLE('',#2360,0.25);
#1003=CIRCLE('',#2362,0.33);
#1004=CIRCLE('',#2363,0.33);
#1005=CIRCLE('',#2386,1.9);
#1006=CIRCLE('',#2388,2.);
#1007=CIRCLE('',#2390,2.);
#1008=CIRCLE('',#2394,0.48);
#1009=CIRCLE('',#2395,0.52);
#1010=CIRCLE('',#2397,2.);
#1011=CIRCLE('',#2399,2.);
#1012=CIRCLE('',#2401,1.);
#1013=CIRCLE('',#2405,0.3933);
#1014=CIRCLE('',#2413,0.3);
#1015=CIRCLE('',#2414,0.3);
#1016=CIRCLE('',#2417,0.3933);
#1017=CIRCLE('',#2419,0.3);
#1018=CIRCLE('',#2422,0.5);
#1019=CIRCLE('',#2428,0.2942);
#1020=CIRCLE('',#2429,0.2942);
#1021=CIRCLE('',#2431,0.24);
#1022=CIRCLE('',#2434,0.475);
#1023=CIRCLE('',#2487,0.21);
#1024=CIRCLE('',#2488,0.21);
#1025=VERTEX_POINT('',#3106);
#1026=VERTEX_POINT('',#3108);
#1027=VERTEX_POINT('',#3112);
#1028=VERTEX_POINT('',#3113);
#1029=VERTEX_POINT('',#3115);
#1030=VERTEX_POINT('',#3117);
#1031=VERTEX_POINT('',#3121);
#1032=VERTEX_POINT('',#3123);
#1033=VERTEX_POINT('',#3127);
#1034=VERTEX_POINT('',#3129);
#1035=VERTEX_POINT('',#3139);
#1036=VERTEX_POINT('',#3140);
#1037=VERTEX_POINT('',#3142);
#1038=VERTEX_POINT('',#3144);
#1039=VERTEX_POINT('',#3148);
#1040=VERTEX_POINT('',#3150);
#1041=VERTEX_POINT('',#3154);
#1042=VERTEX_POINT('',#3156);
#1043=VERTEX_POINT('',#3163);
#1044=VERTEX_POINT('',#3164);
#1045=VERTEX_POINT('',#3166);
#1046=VERTEX_POINT('',#3168);
#1047=VERTEX_POINT('',#3172);
#1048=VERTEX_POINT('',#3174);
#1049=VERTEX_POINT('',#3178);
#1050=VERTEX_POINT('',#3180);
#1051=VERTEX_POINT('',#3190);
#1052=VERTEX_POINT('',#3192);
#1053=VERTEX_POINT('',#3196);
#1054=VERTEX_POINT('',#3198);
#1055=VERTEX_POINT('',#3202);
#1056=VERTEX_POINT('',#3203);
#1057=VERTEX_POINT('',#3205);
#1058=VERTEX_POINT('',#3207);
#1059=VERTEX_POINT('',#3209);
#1060=VERTEX_POINT('',#3213);
#1061=VERTEX_POINT('',#3214);
#1062=VERTEX_POINT('',#3216);
#1063=VERTEX_POINT('',#3218);
#1064=VERTEX_POINT('',#3220);
#1065=VERTEX_POINT('',#3227);
#1066=VERTEX_POINT('',#3229);
#1067=VERTEX_POINT('',#3231);
#1068=VERTEX_POINT('',#3233);
#1069=VERTEX_POINT('',#3236);
#1070=VERTEX_POINT('',#3238);
#1071=VERTEX_POINT('',#3240);
#1072=VERTEX_POINT('',#3242);
#1073=VERTEX_POINT('',#3246);
#1074=VERTEX_POINT('',#3250);
#1075=VERTEX_POINT('',#3254);
#1076=VERTEX_POINT('',#3256);
#1077=VERTEX_POINT('',#3258);
#1078=VERTEX_POINT('',#3260);
#1079=VERTEX_POINT('',#3264);
#1080=VERTEX_POINT('',#3266);
#1081=VERTEX_POINT('',#3269);
#1082=VERTEX_POINT('',#3271);
#1083=VERTEX_POINT('',#3280);
#1084=VERTEX_POINT('',#3281);
#1085=VERTEX_POINT('',#3286);
#1086=VERTEX_POINT('',#3290);
#1087=VERTEX_POINT('',#3296);
#1088=VERTEX_POINT('',#3300);
#1089=VERTEX_POINT('',#3309);
#1090=VERTEX_POINT('',#3312);
#1091=VERTEX_POINT('',#3316);
#1092=VERTEX_POINT('',#3322);
#1093=VERTEX_POINT('',#3324);
#1094=VERTEX_POINT('',#3327);
#1095=VERTEX_POINT('',#3330);
#1096=VERTEX_POINT('',#3334);
#1097=VERTEX_POINT('',#3340);
#1098=VERTEX_POINT('',#3341);
#1099=VERTEX_POINT('',#3343);
#1100=VERTEX_POINT('',#3345);
#1101=VERTEX_POINT('',#3347);
#1102=VERTEX_POINT('',#3349);
#1103=VERTEX_POINT('',#3352);
#1104=VERTEX_POINT('',#3355);
#1105=VERTEX_POINT('',#3356);
#1106=VERTEX_POINT('',#3361);
#1107=VERTEX_POINT('',#3365);
#1108=VERTEX_POINT('',#3369);
#1109=VERTEX_POINT('',#3373);
#1110=VERTEX_POINT('',#3379);
#1111=VERTEX_POINT('',#3381);
#1112=VERTEX_POINT('',#3386);
#1113=VERTEX_POINT('',#3390);
#1114=VERTEX_POINT('',#3395);
#1115=VERTEX_POINT('',#3402);
#1116=VERTEX_POINT('',#3404);
#1117=VERTEX_POINT('',#3408);
#1118=VERTEX_POINT('',#3413);
#1119=VERTEX_POINT('',#3415);
#1120=VERTEX_POINT('',#3417);
#1121=VERTEX_POINT('',#3421);
#1122=VERTEX_POINT('',#3425);
#1123=VERTEX_POINT('',#3429);
#1124=VERTEX_POINT('',#3433);
#1125=VERTEX_POINT('',#3441);
#1126=VERTEX_POINT('',#3443);
#1127=VERTEX_POINT('',#3447);
#1128=VERTEX_POINT('',#3451);
#1129=VERTEX_POINT('',#3455);
#1130=VERTEX_POINT('',#3459);
#1131=VERTEX_POINT('',#3474);
#1132=VERTEX_POINT('',#3475);
#1133=VERTEX_POINT('',#3477);
#1134=VERTEX_POINT('',#3479);
#1135=VERTEX_POINT('',#3483);
#1136=VERTEX_POINT('',#3485);
#1137=VERTEX_POINT('',#3489);
#1138=VERTEX_POINT('',#3491);
#1139=VERTEX_POINT('',#3495);
#1140=VERTEX_POINT('',#3497);
#1141=VERTEX_POINT('',#3501);
#1142=VERTEX_POINT('',#3503);
#1143=VERTEX_POINT('',#3507);
#1144=VERTEX_POINT('',#3509);
#1145=VERTEX_POINT('',#3513);
#1146=VERTEX_POINT('',#3515);
#1147=VERTEX_POINT('',#3519);
#1148=VERTEX_POINT('',#3521);
#1149=VERTEX_POINT('',#3525);
#1150=VERTEX_POINT('',#3527);
#1151=VERTEX_POINT('',#3531);
#1152=VERTEX_POINT('',#3532);
#1153=VERTEX_POINT('',#3534);
#1154=VERTEX_POINT('',#3536);
#1155=VERTEX_POINT('',#3540);
#1156=VERTEX_POINT('',#3542);
#1157=VERTEX_POINT('',#3546);
#1158=VERTEX_POINT('',#3548);
#1159=VERTEX_POINT('',#3552);
#1160=VERTEX_POINT('',#3554);
#1161=VERTEX_POINT('',#3558);
#1162=VERTEX_POINT('',#3560);
#1163=VERTEX_POINT('',#3564);
#1164=VERTEX_POINT('',#3566);
#1165=VERTEX_POINT('',#3570);
#1166=VERTEX_POINT('',#3572);
#1167=VERTEX_POINT('',#3576);
#1168=VERTEX_POINT('',#3578);
#1169=VERTEX_POINT('',#3582);
#1170=VERTEX_POINT('',#3584);
#1171=VERTEX_POINT('',#3588);
#1172=VERTEX_POINT('',#3589);
#1173=VERTEX_POINT('',#3591);
#1174=VERTEX_POINT('',#3593);
#1175=VERTEX_POINT('',#3597);
#1176=VERTEX_POINT('',#3599);
#1177=VERTEX_POINT('',#3603);
#1178=VERTEX_POINT('',#3605);
#1179=VERTEX_POINT('',#3609);
#1180=VERTEX_POINT('',#3611);
#1181=VERTEX_POINT('',#3615);
#1182=VERTEX_POINT('',#3617);
#1183=VERTEX_POINT('',#3621);
#1184=VERTEX_POINT('',#3623);
#1185=VERTEX_POINT('',#3627);
#1186=VERTEX_POINT('',#3629);
#1187=VERTEX_POINT('',#3633);
#1188=VERTEX_POINT('',#3635);
#1189=VERTEX_POINT('',#3639);
#1190=VERTEX_POINT('',#3641);
#1191=VERTEX_POINT('',#3645);
#1192=VERTEX_POINT('',#3646);
#1193=VERTEX_POINT('',#3648);
#1194=VERTEX_POINT('',#3650);
#1195=VERTEX_POINT('',#3654);
#1196=VERTEX_POINT('',#3656);
#1197=VERTEX_POINT('',#3660);
#1198=VERTEX_POINT('',#3662);
#1199=VERTEX_POINT('',#3666);
#1200=VERTEX_POINT('',#3668);
#1201=VERTEX_POINT('',#3672);
#1202=VERTEX_POINT('',#3674);
#1203=VERTEX_POINT('',#3678);
#1204=VERTEX_POINT('',#3680);
#1205=VERTEX_POINT('',#3684);
#1206=VERTEX_POINT('',#3686);
#1207=VERTEX_POINT('',#3690);
#1208=VERTEX_POINT('',#3692);
#1209=VERTEX_POINT('',#3696);
#1210=VERTEX_POINT('',#3698);
#1211=VERTEX_POINT('',#3702);
#1212=VERTEX_POINT('',#3704);
#1213=VERTEX_POINT('',#3708);
#1214=VERTEX_POINT('',#3710);
#1215=VERTEX_POINT('',#3714);
#1216=VERTEX_POINT('',#3716);
#1217=VERTEX_POINT('',#3723);
#1218=VERTEX_POINT('',#3725);
#1219=VERTEX_POINT('',#3732);
#1220=VERTEX_POINT('',#3734);
#1221=EDGE_CURVE('',#1025,#1025,#999,.T.);
#1222=EDGE_CURVE('',#1025,#1026,#471,.T.);
#1223=EDGE_CURVE('',#1026,#1026,#1000,.T.);
#1224=EDGE_CURVE('',#1027,#1028,#472,.T.);
#1225=EDGE_CURVE('',#1028,#1029,#473,.T.);
#1226=EDGE_CURVE('',#1030,#1029,#474,.T.);
#1227=EDGE_CURVE('',#1027,#1030,#475,.T.);
#1228=EDGE_CURVE('',#1031,#1027,#476,.T.);
#1229=EDGE_CURVE('',#1032,#1030,#477,.T.);
#1230=EDGE_CURVE('',#1031,#1032,#478,.T.);
#1231=EDGE_CURVE('',#1033,#1031,#479,.T.);
#1232=EDGE_CURVE('',#1034,#1032,#480,.T.);
#1233=EDGE_CURVE('',#1033,#1034,#481,.T.);
#1234=EDGE_CURVE('',#1028,#1033,#482,.T.);
#1235=EDGE_CURVE('',#1029,#1034,#483,.T.);
#1236=EDGE_CURVE('',#1035,#1036,#484,.T.);
#1237=EDGE_CURVE('',#1037,#1035,#485,.T.);
#1238=EDGE_CURVE('',#1038,#1037,#486,.T.);
#1239=EDGE_CURVE('',#1038,#1036,#487,.T.);
#1240=EDGE_CURVE('',#1036,#1039,#488,.T.);
#1241=EDGE_CURVE('',#1040,#1038,#489,.T.);
#1242=EDGE_CURVE('',#1040,#1039,#490,.T.);
#1243=EDGE_CURVE('',#1039,#1041,#491,.T.);
#1244=EDGE_CURVE('',#1042,#1040,#492,.T.);
#1245=EDGE_CURVE('',#1042,#1041,#493,.T.);
#1246=EDGE_CURVE('',#1041,#1035,#494,.T.);
#1247=EDGE_CURVE('',#1037,#1042,#495,.T.);
#1248=EDGE_CURVE('',#1043,#1044,#496,.T.);
#1249=EDGE_CURVE('',#1044,#1045,#497,.T.);
#1250=EDGE_CURVE('',#1046,#1045,#498,.T.);
#1251=EDGE_CURVE('',#1043,#1046,#499,.T.);
#1252=EDGE_CURVE('',#1047,#1043,#500,.T.);
#1253=EDGE_CURVE('',#1048,#1046,#501,.T.);
#1254=EDGE_CURVE('',#1047,#1048,#502,.T.);
#1255=EDGE_CURVE('',#1049,#1047,#503,.T.);
#1256=EDGE_CURVE('',#1050,#1048,#504,.T.);
#1257=EDGE_CURVE('',#1049,#1050,#505,.T.);
#1258=EDGE_CURVE('',#1044,#1049,#506,.T.);
#1259=EDGE_CURVE('',#1045,#1050,#507,.T.);
#1260=EDGE_CURVE('',#1051,#1051,#1001,.T.);
#1261=EDGE_CURVE('',#1051,#1052,#508,.T.);
#1262=EDGE_CURVE('',#1052,#1052,#1002,.T.);
#1263=EDGE_CURVE('',#1053,#1053,#1003,.T.);
#1264=EDGE_CURVE('',#1053,#1054,#509,.T.);
#1265=EDGE_CURVE('',#1054,#1054,#1004,.T.);
#1266=EDGE_CURVE('',#1055,#1056,#510,.T.);
#1267=EDGE_CURVE('',#1057,#1055,#511,.T.);
#1268=EDGE_CURVE('',#1058,#1057,#512,.T.);
#1269=EDGE_CURVE('',#1059,#1058,#513,.T.);
#1270=EDGE_CURVE('',#1056,#1059,#514,.T.);
#1271=EDGE_CURVE('',#1060,#1061,#515,.T.);
#1272=EDGE_CURVE('',#1062,#1060,#516,.T.);
#1273=EDGE_CURVE('',#1063,#1062,#517,.T.);
#1274=EDGE_CURVE('',#1064,#1063,#518,.T.);
#1275=EDGE_CURVE('',#1061,#1064,#519,.T.);
#1276=EDGE_CURVE('',#1064,#1057,#520,.T.);
#1277=EDGE_CURVE('',#1058,#1063,#521,.T.);
#1278=EDGE_CURVE('',#1055,#1065,#522,.T.);
#1279=EDGE_CURVE('',#1065,#1066,#523,.T.);
#1280=EDGE_CURVE('',#1066,#1067,#524,.T.);
#1281=EDGE_CURVE('',#1067,#1068,#525,.T.);
#1282=EDGE_CURVE('',#1068,#1061,#526,.T.);
#1283=EDGE_CURVE('',#1069,#1064,#527,.T.);
#1284=EDGE_CURVE('',#1070,#1069,#528,.T.);
#1285=EDGE_CURVE('',#1071,#1070,#529,.T.);
#1286=EDGE_CURVE('',#1072,#1071,#530,.T.);
#1287=EDGE_CURVE('',#1057,#1072,#531,.T.);
#1288=EDGE_CURVE('',#1068,#1073,#532,.T.);
#1289=EDGE_CURVE('',#1060,#1073,#533,.T.);
#1290=EDGE_CURVE('',#1074,#1056,#534,.T.);
#1291=EDGE_CURVE('',#1065,#1074,#535,.T.);
#1292=EDGE_CURVE('',#1075,#1062,#536,.T.);
#1293=EDGE_CURVE('',#1076,#1075,#537,.T.);
#1294=EDGE_CURVE('',#1076,#1077,#538,.T.);
#1295=EDGE_CURVE('',#1077,#1078,#539,.T.);
#1296=EDGE_CURVE('',#1059,#1078,#540,.T.);
#1297=EDGE_CURVE('',#1078,#1079,#541,.T.);
#1298=EDGE_CURVE('',#1079,#1080,#542,.T.);
#1299=EDGE_CURVE('',#1080,#1075,#543,.T.);
#1300=EDGE_CURVE('',#1073,#1081,#544,.T.);
#1301=EDGE_CURVE('',#1081,#1082,#545,.T.);
#1302=EDGE_CURVE('',#1082,#1074,#546,.T.);
#1303=EDGE_CURVE('',#1067,#1081,#547,.T.);
#1304=EDGE_CURVE('',#1066,#1082,#548,.T.);
#1305=EDGE_CURVE('',#1083,#1084,#549,.T.);
#1306=EDGE_CURVE('',#1083,#1070,#550,.T.);
#1307=EDGE_CURVE('',#1084,#1069,#551,.T.);
#1308=EDGE_CURVE('',#1084,#1085,#552,.T.);
#1309=EDGE_CURVE('',#1085,#1072,#553,.T.);
#1310=EDGE_CURVE('',#1085,#1086,#554,.T.);
#1311=EDGE_CURVE('',#1086,#1071,#555,.T.);
#1312=EDGE_CURVE('',#1086,#1083,#556,.T.);
#1313=EDGE_CURVE('',#1077,#1087,#557,.T.);
#1314=EDGE_CURVE('',#1087,#1079,#558,.T.);
#1315=EDGE_CURVE('',#1088,#1076,#559,.T.);
#1316=EDGE_CURVE('',#1088,#1080,#560,.T.);
#1317=EDGE_CURVE('',#1087,#1088,#561,.T.);
#1318=EDGE_CURVE('',#1089,#1089,#1005,.T.);
#1319=EDGE_CURVE('',#1090,#1090,#1006,.T.);
#1320=EDGE_CURVE('',#1090,#1089,#562,.T.);
#1321=EDGE_CURVE('',#1091,#1091,#1007,.T.);
#1322=EDGE_CURVE('',#1091,#1090,#563,.T.);
#1323=EDGE_CURVE('',#1092,#1092,#1008,.T.);
#1324=EDGE_CURVE('',#1093,#1092,#1009,.T.);
#1325=EDGE_CURVE('',#1094,#1094,#1010,.T.);
#1326=EDGE_CURVE('',#1095,#1095,#1011,.T.);
#1327=EDGE_CURVE('',#1095,#1094,#564,.T.);
#1328=EDGE_CURVE('',#1096,#1096,#1012,.T.);
#1329=EDGE_CURVE('',#1096,#1095,#565,.T.);
#1330=EDGE_CURVE('',#1097,#1098,#566,.T.);
#1331=EDGE_CURVE('',#1098,#1099,#567,.T.);
#1332=EDGE_CURVE('',#1099,#1100,#568,.T.);
#1333=EDGE_CURVE('',#1100,#1101,#569,.T.);
#1334=EDGE_CURVE('',#1101,#1102,#570,.T.);
#1335=EDGE_CURVE('',#1102,#1097,#571,.T.);
#1336=EDGE_CURVE('',#1103,#1103,#1013,.F.);
#1337=EDGE_CURVE('',#1104,#1105,#572,.T.);
#1338=EDGE_CURVE('',#1105,#1097,#573,.T.);
#1339=EDGE_CURVE('',#1104,#1102,#574,.T.);
#1340=EDGE_CURVE('',#1106,#1104,#575,.T.);
#1341=EDGE_CURVE('',#1106,#1101,#576,.T.);
#1342=EDGE_CURVE('',#1107,#1106,#577,.T.);
#1343=EDGE_CURVE('',#1107,#1100,#578,.T.);
#1344=EDGE_CURVE('',#1108,#1107,#579,.T.);
#1345=EDGE_CURVE('',#1108,#1099,#580,.T.);
#1346=EDGE_CURVE('',#1109,#1108,#581,.T.);
#1347=EDGE_CURVE('',#1109,#1098,#582,.T.);
#1348=EDGE_CURVE('',#1105,#1109,#583,.T.);
#1349=EDGE_CURVE('',#1110,#1110,#1014,.T.);
#1350=EDGE_CURVE('',#1110,#1111,#584,.T.);
#1351=EDGE_CURVE('',#1111,#1111,#1015,.T.);
#1352=EDGE_CURVE('',#1112,#1112,#1016,.F.);
#1353=EDGE_CURVE('',#1112,#1103,#585,.T.);
#1354=EDGE_CURVE('',#1113,#1113,#1017,.T.);
#1355=EDGE_CURVE('',#1113,#1112,#586,.T.);
#1356=EDGE_CURVE('',#1111,#1114,#1018,.T.);
#1357=EDGE_CURVE('',#1115,#1115,#1019,.F.);
#1358=EDGE_CURVE('',#1115,#1116,#587,.T.);
#1359=EDGE_CURVE('',#1116,#1116,#1020,.F.);
#1360=EDGE_CURVE('',#1117,#1117,#1021,.T.);
#1361=EDGE_CURVE('',#1117,#1115,#588,.T.);
#1362=EDGE_CURVE('',#1118,#1118,#1022,.T.);
#1363=EDGE_CURVE('',#1118,#1119,#589,.T.);
#1364=EDGE_CURVE('',#1120,#1119,#11,.T.);
#1365=EDGE_CURVE('',#1121,#1120,#12,.T.);
#1366=EDGE_CURVE('',#1122,#1121,#13,.T.);
#1367=EDGE_CURVE('',#1123,#1122,#14,.T.);
#1368=EDGE_CURVE('',#1124,#1123,#15,.T.);
#1369=EDGE_CURVE('',#1119,#1124,#16,.T.);
#1370=EDGE_CURVE('',#1125,#1123,#590,.T.);
#1371=EDGE_CURVE('',#1125,#1126,#591,.T.);
#1372=EDGE_CURVE('',#1126,#1124,#592,.T.);
#1373=EDGE_CURVE('',#1127,#1122,#593,.T.);
#1374=EDGE_CURVE('',#1127,#1125,#594,.T.);
#1375=EDGE_CURVE('',#1128,#1121,#595,.T.);
#1376=EDGE_CURVE('',#1128,#1127,#596,.T.);
#1377=EDGE_CURVE('',#1129,#1120,#597,.T.);
#1378=EDGE_CURVE('',#1129,#1128,#598,.T.);
#1379=EDGE_CURVE('',#1130,#1119,#599,.T.);
#1380=EDGE_CURVE('',#1130,#1129,#600,.T.);
#1381=EDGE_CURVE('',#1126,#1130,#601,.T.);
#1382=EDGE_CURVE('',#1131,#1132,#602,.T.);
#1383=EDGE_CURVE('',#1131,#1133,#603,.T.);
#1384=EDGE_CURVE('',#1134,#1133,#604,.T.);
#1385=EDGE_CURVE('',#1132,#1134,#605,.T.);
#1386=EDGE_CURVE('',#1135,#1131,#606,.T.);
#1387=EDGE_CURVE('',#1135,#1136,#607,.T.);
#1388=EDGE_CURVE('',#1133,#1136,#608,.T.);
#1389=EDGE_CURVE('',#1137,#1135,#609,.T.);
#1390=EDGE_CURVE('',#1137,#1138,#610,.T.);
#1391=EDGE_CURVE('',#1136,#1138,#611,.T.);
#1392=EDGE_CURVE('',#1139,#1137,#612,.T.);
#1393=EDGE_CURVE('',#1139,#1140,#613,.T.);
#1394=EDGE_CURVE('',#1138,#1140,#614,.T.);
#1395=EDGE_CURVE('',#1141,#1139,#615,.T.);
#1396=EDGE_CURVE('',#1141,#1142,#616,.T.);
#1397=EDGE_CURVE('',#1140,#1142,#617,.T.);
#1398=EDGE_CURVE('',#1143,#1141,#618,.T.);
#1399=EDGE_CURVE('',#1143,#1144,#619,.T.);
#1400=EDGE_CURVE('',#1142,#1144,#620,.T.);
#1401=EDGE_CURVE('',#1145,#1143,#621,.T.);
#1402=EDGE_CURVE('',#1145,#1146,#622,.T.);
#1403=EDGE_CURVE('',#1144,#1146,#623,.T.);
#1404=EDGE_CURVE('',#1147,#1145,#624,.T.);
#1405=EDGE_CURVE('',#1147,#1148,#625,.T.);
#1406=EDGE_CURVE('',#1146,#1148,#626,.T.);
#1407=EDGE_CURVE('',#1149,#1147,#627,.T.);
#1408=EDGE_CURVE('',#1150,#1149,#628,.T.);
#1409=EDGE_CURVE('',#1148,#1150,#629,.T.);
#1410=EDGE_CURVE('',#1151,#1152,#630,.T.);
#1411=EDGE_CURVE('',#1151,#1153,#631,.T.);
#1412=EDGE_CURVE('',#1154,#1153,#632,.T.);
#1413=EDGE_CURVE('',#1152,#1154,#633,.T.);
#1414=EDGE_CURVE('',#1155,#1151,#634,.T.);
#1415=EDGE_CURVE('',#1155,#1156,#635,.T.);
#1416=EDGE_CURVE('',#1153,#1156,#636,.T.);
#1417=EDGE_CURVE('',#1157,#1155,#637,.T.);
#1418=EDGE_CURVE('',#1157,#1158,#638,.T.);
#1419=EDGE_CURVE('',#1156,#1158,#639,.T.);
#1420=EDGE_CURVE('',#1159,#1157,#640,.T.);
#1421=EDGE_CURVE('',#1159,#1160,#641,.T.);
#1422=EDGE_CURVE('',#1158,#1160,#642,.T.);
#1423=EDGE_CURVE('',#1161,#1159,#643,.T.);
#1424=EDGE_CURVE('',#1161,#1162,#644,.T.);
#1425=EDGE_CURVE('',#1160,#1162,#645,.T.);
#1426=EDGE_CURVE('',#1163,#1161,#646,.T.);
#1427=EDGE_CURVE('',#1163,#1164,#647,.T.);
#1428=EDGE_CURVE('',#1162,#1164,#648,.T.);
#1429=EDGE_CURVE('',#1165,#1163,#649,.T.);
#1430=EDGE_CURVE('',#1165,#1166,#650,.T.);
#1431=EDGE_CURVE('',#1164,#1166,#651,.T.);
#1432=EDGE_CURVE('',#1167,#1165,#652,.T.);
#1433=EDGE_CURVE('',#1167,#1168,#653,.T.);
#1434=EDGE_CURVE('',#1166,#1168,#654,.T.);
#1435=EDGE_CURVE('',#1169,#1167,#655,.T.);
#1436=EDGE_CURVE('',#1170,#1169,#656,.T.);
#1437=EDGE_CURVE('',#1168,#1170,#657,.T.);
#1438=EDGE_CURVE('',#1171,#1172,#658,.T.);
#1439=EDGE_CURVE('',#1171,#1173,#659,.T.);
#1440=EDGE_CURVE('',#1174,#1173,#660,.T.);
#1441=EDGE_CURVE('',#1172,#1174,#661,.T.);
#1442=EDGE_CURVE('',#1175,#1171,#662,.T.);
#1443=EDGE_CURVE('',#1175,#1176,#663,.T.);
#1444=EDGE_CURVE('',#1173,#1176,#664,.T.);
#1445=EDGE_CURVE('',#1177,#1175,#665,.T.);
#1446=EDGE_CURVE('',#1177,#1178,#666,.T.);
#1447=EDGE_CURVE('',#1176,#1178,#667,.T.);
#1448=EDGE_CURVE('',#1179,#1177,#668,.T.);
#1449=EDGE_CURVE('',#1179,#1180,#669,.T.);
#1450=EDGE_CURVE('',#1178,#1180,#670,.T.);
#1451=EDGE_CURVE('',#1181,#1179,#671,.T.);
#1452=EDGE_CURVE('',#1181,#1182,#672,.T.);
#1453=EDGE_CURVE('',#1180,#1182,#673,.T.);
#1454=EDGE_CURVE('',#1183,#1181,#674,.T.);
#1455=EDGE_CURVE('',#1183,#1184,#675,.T.);
#1456=EDGE_CURVE('',#1182,#1184,#676,.T.);
#1457=EDGE_CURVE('',#1185,#1183,#677,.T.);
#1458=EDGE_CURVE('',#1185,#1186,#678,.T.);
#1459=EDGE_CURVE('',#1184,#1186,#679,.T.);
#1460=EDGE_CURVE('',#1187,#1185,#680,.T.);
#1461=EDGE_CURVE('',#1187,#1188,#681,.T.);
#1462=EDGE_CURVE('',#1186,#1188,#682,.T.);
#1463=EDGE_CURVE('',#1189,#1187,#683,.T.);
#1464=EDGE_CURVE('',#1190,#1189,#684,.T.);
#1465=EDGE_CURVE('',#1188,#1190,#685,.T.);
#1466=EDGE_CURVE('',#1191,#1192,#686,.T.);
#1467=EDGE_CURVE('',#1191,#1193,#687,.T.);
#1468=EDGE_CURVE('',#1194,#1193,#688,.T.);
#1469=EDGE_CURVE('',#1192,#1194,#689,.T.);
#1470=EDGE_CURVE('',#1195,#1191,#690,.T.);
#1471=EDGE_CURVE('',#1195,#1196,#691,.T.);
#1472=EDGE_CURVE('',#1193,#1196,#692,.T.);
#1473=EDGE_CURVE('',#1197,#1195,#693,.T.);
#1474=EDGE_CURVE('',#1197,#1198,#694,.T.);
#1475=EDGE_CURVE('',#1196,#1198,#695,.T.);
#1476=EDGE_CURVE('',#1199,#1197,#696,.T.);
#1477=EDGE_CURVE('',#1199,#1200,#697,.T.);
#1478=EDGE_CURVE('',#1198,#1200,#698,.T.);
#1479=EDGE_CURVE('',#1201,#1199,#699,.T.);
#1480=EDGE_CURVE('',#1201,#1202,#700,.T.);
#1481=EDGE_CURVE('',#1200,#1202,#701,.T.);
#1482=EDGE_CURVE('',#1203,#1201,#702,.T.);
#1483=EDGE_CURVE('',#1203,#1204,#703,.T.);
#1484=EDGE_CURVE('',#1202,#1204,#704,.T.);
#1485=EDGE_CURVE('',#1205,#1203,#705,.T.);
#1486=EDGE_CURVE('',#1205,#1206,#706,.T.);
#1487=EDGE_CURVE('',#1204,#1206,#707,.T.);
#1488=EDGE_CURVE('',#1207,#1205,#708,.T.);
#1489=EDGE_CURVE('',#1207,#1208,#709,.T.);
#1490=EDGE_CURVE('',#1206,#1208,#710,.T.);
#1491=EDGE_CURVE('',#1209,#1207,#711,.T.);
#1492=EDGE_CURVE('',#1210,#1209,#712,.T.);
#1493=EDGE_CURVE('',#1208,#1210,#713,.T.);
#1494=EDGE_CURVE('',#1211,#1211,#1023,.T.);
#1495=EDGE_CURVE('',#1211,#1212,#714,.T.);
#1496=EDGE_CURVE('',#1212,#1212,#1024,.T.);
#1497=EDGE_CURVE('',#1149,#1213,#715,.T.);
#1498=EDGE_CURVE('',#1213,#1214,#716,.T.);
#1499=EDGE_CURVE('',#1150,#1214,#717,.T.);
#1500=EDGE_CURVE('',#1215,#1134,#718,.T.);
#1501=EDGE_CURVE('',#1216,#1215,#719,.T.);
#1502=EDGE_CURVE('',#1216,#1132,#720,.T.);
#1503=EDGE_CURVE('',#1169,#1216,#721,.T.);
#1504=EDGE_CURVE('',#1170,#1215,#722,.T.);
#1505=EDGE_CURVE('',#1217,#1154,#723,.T.);
#1506=EDGE_CURVE('',#1218,#1217,#724,.T.);
#1507=EDGE_CURVE('',#1218,#1152,#725,.T.);
#1508=EDGE_CURVE('',#1189,#1218,#726,.T.);
#1509=EDGE_CURVE('',#1190,#1217,#727,.T.);
#1510=EDGE_CURVE('',#1219,#1174,#728,.T.);
#1511=EDGE_CURVE('',#1220,#1219,#729,.T.);
#1512=EDGE_CURVE('',#1220,#1172,#730,.T.);
#1513=EDGE_CURVE('',#1209,#1220,#731,.T.);
#1514=EDGE_CURVE('',#1210,#1219,#732,.T.);
#1515=EDGE_CURVE('',#1214,#1194,#733,.T.);
#1516=EDGE_CURVE('',#1213,#1192,#734,.T.);
#1517=ORIENTED_EDGE('',*,*,#1221,.F.);
#1518=ORIENTED_EDGE('',*,*,#1222,.T.);
#1519=ORIENTED_EDGE('',*,*,#1223,.F.);
#1520=ORIENTED_EDGE('',*,*,#1222,.F.);
#1521=ORIENTED_EDGE('',*,*,#1224,.T.);
#1522=ORIENTED_EDGE('',*,*,#1225,.T.);
#1523=ORIENTED_EDGE('',*,*,#1226,.F.);
#1524=ORIENTED_EDGE('',*,*,#1227,.F.);
#1525=ORIENTED_EDGE('',*,*,#1228,.T.);
#1526=ORIENTED_EDGE('',*,*,#1227,.T.);
#1527=ORIENTED_EDGE('',*,*,#1229,.F.);
#1528=ORIENTED_EDGE('',*,*,#1230,.F.);
#1529=ORIENTED_EDGE('',*,*,#1231,.T.);
#1530=ORIENTED_EDGE('',*,*,#1230,.T.);
#1531=ORIENTED_EDGE('',*,*,#1232,.F.);
#1532=ORIENTED_EDGE('',*,*,#1233,.F.);
#1533=ORIENTED_EDGE('',*,*,#1234,.T.);
#1534=ORIENTED_EDGE('',*,*,#1233,.T.);
#1535=ORIENTED_EDGE('',*,*,#1235,.F.);
#1536=ORIENTED_EDGE('',*,*,#1225,.F.);
#1537=ORIENTED_EDGE('',*,*,#1235,.T.);
#1538=ORIENTED_EDGE('',*,*,#1232,.T.);
#1539=ORIENTED_EDGE('',*,*,#1229,.T.);
#1540=ORIENTED_EDGE('',*,*,#1226,.T.);
#1541=ORIENTED_EDGE('',*,*,#1223,.T.);
#1542=ORIENTED_EDGE('',*,*,#1234,.F.);
#1543=ORIENTED_EDGE('',*,*,#1224,.F.);
#1544=ORIENTED_EDGE('',*,*,#1228,.F.);
#1545=ORIENTED_EDGE('',*,*,#1231,.F.);
#1546=ORIENTED_EDGE('',*,*,#1221,.T.);
#1547=ORIENTED_EDGE('',*,*,#1236,.F.);
#1548=ORIENTED_EDGE('',*,*,#1237,.F.);
#1549=ORIENTED_EDGE('',*,*,#1238,.F.);
#1550=ORIENTED_EDGE('',*,*,#1239,.T.);
#1551=ORIENTED_EDGE('',*,*,#1240,.F.);
#1552=ORIENTED_EDGE('',*,*,#1239,.F.);
#1553=ORIENTED_EDGE('',*,*,#1241,.F.);
#1554=ORIENTED_EDGE('',*,*,#1242,.T.);
#1555=ORIENTED_EDGE('',*,*,#1243,.F.);
#1556=ORIENTED_EDGE('',*,*,#1242,.F.);
#1557=ORIENTED_EDGE('',*,*,#1244,.F.);
#1558=ORIENTED_EDGE('',*,*,#1245,.T.);
#1559=ORIENTED_EDGE('',*,*,#1246,.F.);
#1560=ORIENTED_EDGE('',*,*,#1245,.F.);
#1561=ORIENTED_EDGE('',*,*,#1247,.F.);
#1562=ORIENTED_EDGE('',*,*,#1237,.T.);
#1563=ORIENTED_EDGE('',*,*,#1248,.T.);
#1564=ORIENTED_EDGE('',*,*,#1249,.T.);
#1565=ORIENTED_EDGE('',*,*,#1250,.F.);
#1566=ORIENTED_EDGE('',*,*,#1251,.F.);
#1567=ORIENTED_EDGE('',*,*,#1252,.T.);
#1568=ORIENTED_EDGE('',*,*,#1251,.T.);
#1569=ORIENTED_EDGE('',*,*,#1253,.F.);
#1570=ORIENTED_EDGE('',*,*,#1254,.F.);
#1571=ORIENTED_EDGE('',*,*,#1255,.T.);
#1572=ORIENTED_EDGE('',*,*,#1254,.T.);
#1573=ORIENTED_EDGE('',*,*,#1256,.F.);
#1574=ORIENTED_EDGE('',*,*,#1257,.F.);
#1575=ORIENTED_EDGE('',*,*,#1258,.T.);
#1576=ORIENTED_EDGE('',*,*,#1257,.T.);
#1577=ORIENTED_EDGE('',*,*,#1259,.F.);
#1578=ORIENTED_EDGE('',*,*,#1249,.F.);
#1579=ORIENTED_EDGE('',*,*,#1259,.T.);
#1580=ORIENTED_EDGE('',*,*,#1256,.T.);
#1581=ORIENTED_EDGE('',*,*,#1253,.T.);
#1582=ORIENTED_EDGE('',*,*,#1250,.T.);
#1583=ORIENTED_EDGE('',*,*,#1243,.T.);
#1584=ORIENTED_EDGE('',*,*,#1246,.T.);
#1585=ORIENTED_EDGE('',*,*,#1236,.T.);
#1586=ORIENTED_EDGE('',*,*,#1240,.T.);
#1587=ORIENTED_EDGE('',*,*,#1258,.F.);
#1588=ORIENTED_EDGE('',*,*,#1248,.F.);
#1589=ORIENTED_EDGE('',*,*,#1252,.F.);
#1590=ORIENTED_EDGE('',*,*,#1255,.F.);
#1591=ORIENTED_EDGE('',*,*,#1244,.T.);
#1592=ORIENTED_EDGE('',*,*,#1241,.T.);
#1593=ORIENTED_EDGE('',*,*,#1238,.T.);
#1594=ORIENTED_EDGE('',*,*,#1247,.T.);
#1595=ORIENTED_EDGE('',*,*,#1260,.F.);
#1596=ORIENTED_EDGE('',*,*,#1261,.T.);
#1597=ORIENTED_EDGE('',*,*,#1262,.F.);
#1598=ORIENTED_EDGE('',*,*,#1261,.F.);
#1599=ORIENTED_EDGE('',*,*,#1263,.F.);
#1600=ORIENTED_EDGE('',*,*,#1264,.T.);
#1601=ORIENTED_EDGE('',*,*,#1265,.F.);
#1602=ORIENTED_EDGE('',*,*,#1264,.F.);
#1603=ORIENTED_EDGE('',*,*,#1266,.F.);
#1604=ORIENTED_EDGE('',*,*,#1267,.F.);
#1605=ORIENTED_EDGE('',*,*,#1268,.F.);
#1606=ORIENTED_EDGE('',*,*,#1269,.F.);
#1607=ORIENTED_EDGE('',*,*,#1270,.F.);
#1608=ORIENTED_EDGE('',*,*,#1260,.T.);
#1609=ORIENTED_EDGE('',*,*,#1271,.F.);
#1610=ORIENTED_EDGE('',*,*,#1272,.F.);
#1611=ORIENTED_EDGE('',*,*,#1273,.F.);
#1612=ORIENTED_EDGE('',*,*,#1274,.F.);
#1613=ORIENTED_EDGE('',*,*,#1275,.F.);
#1614=ORIENTED_EDGE('',*,*,#1265,.T.);
#1615=ORIENTED_EDGE('',*,*,#1276,.F.);
#1616=ORIENTED_EDGE('',*,*,#1274,.T.);
#1617=ORIENTED_EDGE('',*,*,#1277,.F.);
#1618=ORIENTED_EDGE('',*,*,#1268,.T.);
#1619=ORIENTED_EDGE('',*,*,#1267,.T.);
#1620=ORIENTED_EDGE('',*,*,#1278,.T.);
#1621=ORIENTED_EDGE('',*,*,#1279,.T.);
#1622=ORIENTED_EDGE('',*,*,#1280,.T.);
#1623=ORIENTED_EDGE('',*,*,#1281,.T.);
#1624=ORIENTED_EDGE('',*,*,#1282,.T.);
#1625=ORIENTED_EDGE('',*,*,#1275,.T.);
#1626=ORIENTED_EDGE('',*,*,#1283,.F.);
#1627=ORIENTED_EDGE('',*,*,#1284,.F.);
#1628=ORIENTED_EDGE('',*,*,#1285,.F.);
#1629=ORIENTED_EDGE('',*,*,#1286,.F.);
#1630=ORIENTED_EDGE('',*,*,#1287,.F.);
#1631=ORIENTED_EDGE('',*,*,#1271,.T.);
#1632=ORIENTED_EDGE('',*,*,#1282,.F.);
#1633=ORIENTED_EDGE('',*,*,#1288,.T.);
#1634=ORIENTED_EDGE('',*,*,#1289,.F.);
#1635=ORIENTED_EDGE('',*,*,#1266,.T.);
#1636=ORIENTED_EDGE('',*,*,#1290,.F.);
#1637=ORIENTED_EDGE('',*,*,#1291,.F.);
#1638=ORIENTED_EDGE('',*,*,#1278,.F.);
#1639=ORIENTED_EDGE('',*,*,#1269,.T.);
#1640=ORIENTED_EDGE('',*,*,#1277,.T.);
#1641=ORIENTED_EDGE('',*,*,#1273,.T.);
#1642=ORIENTED_EDGE('',*,*,#1292,.F.);
#1643=ORIENTED_EDGE('',*,*,#1293,.F.);
#1644=ORIENTED_EDGE('',*,*,#1294,.T.);
#1645=ORIENTED_EDGE('',*,*,#1295,.T.);
#1646=ORIENTED_EDGE('',*,*,#1296,.F.);
#1647=ORIENTED_EDGE('',*,*,#1270,.T.);
#1648=ORIENTED_EDGE('',*,*,#1296,.T.);
#1649=ORIENTED_EDGE('',*,*,#1297,.T.);
#1650=ORIENTED_EDGE('',*,*,#1298,.T.);
#1651=ORIENTED_EDGE('',*,*,#1299,.T.);
#1652=ORIENTED_EDGE('',*,*,#1292,.T.);
#1653=ORIENTED_EDGE('',*,*,#1272,.T.);
#1654=ORIENTED_EDGE('',*,*,#1289,.T.);
#1655=ORIENTED_EDGE('',*,*,#1300,.T.);
#1656=ORIENTED_EDGE('',*,*,#1301,.T.);
#1657=ORIENTED_EDGE('',*,*,#1302,.T.);
#1658=ORIENTED_EDGE('',*,*,#1290,.T.);
#1659=ORIENTED_EDGE('',*,*,#1281,.F.);
#1660=ORIENTED_EDGE('',*,*,#1303,.T.);
#1661=ORIENTED_EDGE('',*,*,#1300,.F.);
#1662=ORIENTED_EDGE('',*,*,#1288,.F.);
#1663=ORIENTED_EDGE('',*,*,#1279,.F.);
#1664=ORIENTED_EDGE('',*,*,#1291,.T.);
#1665=ORIENTED_EDGE('',*,*,#1302,.F.);
#1666=ORIENTED_EDGE('',*,*,#1304,.F.);
#1667=ORIENTED_EDGE('',*,*,#1280,.F.);
#1668=ORIENTED_EDGE('',*,*,#1304,.T.);
#1669=ORIENTED_EDGE('',*,*,#1301,.F.);
#1670=ORIENTED_EDGE('',*,*,#1303,.F.);
#1671=ORIENTED_EDGE('',*,*,#1305,.F.);
#1672=ORIENTED_EDGE('',*,*,#1306,.T.);
#1673=ORIENTED_EDGE('',*,*,#1284,.T.);
#1674=ORIENTED_EDGE('',*,*,#1307,.F.);
#1675=ORIENTED_EDGE('',*,*,#1308,.F.);
#1676=ORIENTED_EDGE('',*,*,#1307,.T.);
#1677=ORIENTED_EDGE('',*,*,#1283,.T.);
#1678=ORIENTED_EDGE('',*,*,#1276,.T.);
#1679=ORIENTED_EDGE('',*,*,#1287,.T.);
#1680=ORIENTED_EDGE('',*,*,#1309,.F.);
#1681=ORIENTED_EDGE('',*,*,#1310,.F.);
#1682=ORIENTED_EDGE('',*,*,#1309,.T.);
#1683=ORIENTED_EDGE('',*,*,#1286,.T.);
#1684=ORIENTED_EDGE('',*,*,#1311,.F.);
#1685=ORIENTED_EDGE('',*,*,#1312,.F.);
#1686=ORIENTED_EDGE('',*,*,#1311,.T.);
#1687=ORIENTED_EDGE('',*,*,#1285,.T.);
#1688=ORIENTED_EDGE('',*,*,#1306,.F.);
#1689=ORIENTED_EDGE('',*,*,#1313,.T.);
#1690=ORIENTED_EDGE('',*,*,#1314,.T.);
#1691=ORIENTED_EDGE('',*,*,#1297,.F.);
#1692=ORIENTED_EDGE('',*,*,#1295,.F.);
#1693=ORIENTED_EDGE('',*,*,#1262,.T.);
#1694=ORIENTED_EDGE('',*,*,#1315,.T.);
#1695=ORIENTED_EDGE('',*,*,#1293,.T.);
#1696=ORIENTED_EDGE('',*,*,#1299,.F.);
#1697=ORIENTED_EDGE('',*,*,#1316,.F.);
#1698=ORIENTED_EDGE('',*,*,#1263,.T.);
#1699=ORIENTED_EDGE('',*,*,#1317,.T.);
#1700=ORIENTED_EDGE('',*,*,#1316,.T.);
#1701=ORIENTED_EDGE('',*,*,#1298,.F.);
#1702=ORIENTED_EDGE('',*,*,#1314,.F.);
#1703=ORIENTED_EDGE('',*,*,#1317,.F.);
#1704=ORIENTED_EDGE('',*,*,#1313,.F.);
#1705=ORIENTED_EDGE('',*,*,#1294,.F.);
#1706=ORIENTED_EDGE('',*,*,#1315,.F.);
#1707=ORIENTED_EDGE('',*,*,#1310,.T.);
#1708=ORIENTED_EDGE('',*,*,#1312,.T.);
#1709=ORIENTED_EDGE('',*,*,#1305,.T.);
#1710=ORIENTED_EDGE('',*,*,#1308,.T.);
#1711=ORIENTED_EDGE('',*,*,#1318,.F.);
#1712=ORIENTED_EDGE('',*,*,#1319,.F.);
#1713=ORIENTED_EDGE('',*,*,#1320,.T.);
#1714=ORIENTED_EDGE('',*,*,#1318,.T.);
#1715=ORIENTED_EDGE('',*,*,#1320,.F.);
#1716=ORIENTED_EDGE('',*,*,#1321,.F.);
#1717=ORIENTED_EDGE('',*,*,#1322,.T.);
#1718=ORIENTED_EDGE('',*,*,#1319,.T.);
#1719=ORIENTED_EDGE('',*,*,#1322,.F.);
#1720=ORIENTED_EDGE('',*,*,#1321,.T.);
#1721=ORIENTED_EDGE('',*,*,#1323,.F.);
#1722=ORIENTED_EDGE('',*,*,#1324,.F.);
#1723=ORIENTED_EDGE('',*,*,#1324,.T.);
#1724=ORIENTED_EDGE('',*,*,#1325,.F.);
#1725=ORIENTED_EDGE('',*,*,#1326,.F.);
#1726=ORIENTED_EDGE('',*,*,#1327,.T.);
#1727=ORIENTED_EDGE('',*,*,#1325,.T.);
#1728=ORIENTED_EDGE('',*,*,#1327,.F.);
#1729=ORIENTED_EDGE('',*,*,#1328,.F.);
#1730=ORIENTED_EDGE('',*,*,#1329,.T.);
#1731=ORIENTED_EDGE('',*,*,#1326,.T.);
#1732=ORIENTED_EDGE('',*,*,#1329,.F.);
#1733=ORIENTED_EDGE('',*,*,#1328,.T.);
#1734=ORIENTED_EDGE('',*,*,#1323,.T.);
#1735=ORIENTED_EDGE('',*,*,#1330,.T.);
#1736=ORIENTED_EDGE('',*,*,#1331,.T.);
#1737=ORIENTED_EDGE('',*,*,#1332,.T.);
#1738=ORIENTED_EDGE('',*,*,#1333,.T.);
#1739=ORIENTED_EDGE('',*,*,#1334,.T.);
#1740=ORIENTED_EDGE('',*,*,#1335,.T.);
#1741=ORIENTED_EDGE('',*,*,#1336,.F.);
#1742=ORIENTED_EDGE('',*,*,#1337,.T.);
#1743=ORIENTED_EDGE('',*,*,#1338,.T.);
#1744=ORIENTED_EDGE('',*,*,#1335,.F.);
#1745=ORIENTED_EDGE('',*,*,#1339,.F.);
#1746=ORIENTED_EDGE('',*,*,#1340,.T.);
#1747=ORIENTED_EDGE('',*,*,#1339,.T.);
#1748=ORIENTED_EDGE('',*,*,#1334,.F.);
#1749=ORIENTED_EDGE('',*,*,#1341,.F.);
#1750=ORIENTED_EDGE('',*,*,#1342,.T.);
#1751=ORIENTED_EDGE('',*,*,#1341,.T.);
#1752=ORIENTED_EDGE('',*,*,#1333,.F.);
#1753=ORIENTED_EDGE('',*,*,#1343,.F.);
#1754=ORIENTED_EDGE('',*,*,#1344,.T.);
#1755=ORIENTED_EDGE('',*,*,#1343,.T.);
#1756=ORIENTED_EDGE('',*,*,#1332,.F.);
#1757=ORIENTED_EDGE('',*,*,#1345,.F.);
#1758=ORIENTED_EDGE('',*,*,#1346,.T.);
#1759=ORIENTED_EDGE('',*,*,#1345,.T.);
#1760=ORIENTED_EDGE('',*,*,#1331,.F.);
#1761=ORIENTED_EDGE('',*,*,#1347,.F.);
#1762=ORIENTED_EDGE('',*,*,#1348,.T.);
#1763=ORIENTED_EDGE('',*,*,#1347,.T.);
#1764=ORIENTED_EDGE('',*,*,#1330,.F.);
#1765=ORIENTED_EDGE('',*,*,#1338,.F.);
#1766=ORIENTED_EDGE('',*,*,#1349,.F.);
#1767=ORIENTED_EDGE('',*,*,#1350,.T.);
#1768=ORIENTED_EDGE('',*,*,#1351,.F.);
#1769=ORIENTED_EDGE('',*,*,#1350,.F.);
#1770=ORIENTED_EDGE('',*,*,#1348,.F.);
#1771=ORIENTED_EDGE('',*,*,#1337,.F.);
#1772=ORIENTED_EDGE('',*,*,#1340,.F.);
#1773=ORIENTED_EDGE('',*,*,#1342,.F.);
#1774=ORIENTED_EDGE('',*,*,#1344,.F.);
#1775=ORIENTED_EDGE('',*,*,#1346,.F.);
#1776=ORIENTED_EDGE('',*,*,#1349,.T.);
#1777=ORIENTED_EDGE('',*,*,#1352,.F.);
#1778=ORIENTED_EDGE('',*,*,#1353,.T.);
#1779=ORIENTED_EDGE('',*,*,#1336,.T.);
#1780=ORIENTED_EDGE('',*,*,#1353,.F.);
#1781=ORIENTED_EDGE('',*,*,#1354,.F.);
#1782=ORIENTED_EDGE('',*,*,#1355,.T.);
#1783=ORIENTED_EDGE('',*,*,#1352,.T.);
#1784=ORIENTED_EDGE('',*,*,#1355,.F.);
#1785=ORIENTED_EDGE('',*,*,#1354,.T.);
#1786=ORIENTED_EDGE('',*,*,#1351,.T.);
#1787=ORIENTED_EDGE('',*,*,#1356,.T.);
#1788=ORIENTED_EDGE('',*,*,#1356,.F.);
#1789=ORIENTED_EDGE('',*,*,#1357,.F.);
#1790=ORIENTED_EDGE('',*,*,#1358,.T.);
#1791=ORIENTED_EDGE('',*,*,#1359,.F.);
#1792=ORIENTED_EDGE('',*,*,#1358,.F.);
#1793=ORIENTED_EDGE('',*,*,#1360,.F.);
#1794=ORIENTED_EDGE('',*,*,#1361,.T.);
#1795=ORIENTED_EDGE('',*,*,#1357,.T.);
#1796=ORIENTED_EDGE('',*,*,#1361,.F.);
#1797=ORIENTED_EDGE('',*,*,#1360,.T.);
#1798=ORIENTED_EDGE('',*,*,#1362,.F.);
#1799=ORIENTED_EDGE('',*,*,#1363,.T.);
#1800=ORIENTED_EDGE('',*,*,#1364,.F.);
#1801=ORIENTED_EDGE('',*,*,#1365,.F.);
#1802=ORIENTED_EDGE('',*,*,#1366,.F.);
#1803=ORIENTED_EDGE('',*,*,#1367,.F.);
#1804=ORIENTED_EDGE('',*,*,#1368,.F.);
#1805=ORIENTED_EDGE('',*,*,#1369,.F.);
#1806=ORIENTED_EDGE('',*,*,#1363,.F.);
#1807=ORIENTED_EDGE('',*,*,#1368,.T.);
#1808=ORIENTED_EDGE('',*,*,#1370,.F.);
#1809=ORIENTED_EDGE('',*,*,#1371,.T.);
#1810=ORIENTED_EDGE('',*,*,#1372,.T.);
#1811=ORIENTED_EDGE('',*,*,#1367,.T.);
#1812=ORIENTED_EDGE('',*,*,#1373,.F.);
#1813=ORIENTED_EDGE('',*,*,#1374,.T.);
#1814=ORIENTED_EDGE('',*,*,#1370,.T.);
#1815=ORIENTED_EDGE('',*,*,#1366,.T.);
#1816=ORIENTED_EDGE('',*,*,#1375,.F.);
#1817=ORIENTED_EDGE('',*,*,#1376,.T.);
#1818=ORIENTED_EDGE('',*,*,#1373,.T.);
#1819=ORIENTED_EDGE('',*,*,#1365,.T.);
#1820=ORIENTED_EDGE('',*,*,#1377,.F.);
#1821=ORIENTED_EDGE('',*,*,#1378,.T.);
#1822=ORIENTED_EDGE('',*,*,#1375,.T.);
#1823=ORIENTED_EDGE('',*,*,#1364,.T.);
#1824=ORIENTED_EDGE('',*,*,#1379,.F.);
#1825=ORIENTED_EDGE('',*,*,#1380,.T.);
#1826=ORIENTED_EDGE('',*,*,#1377,.T.);
#1827=ORIENTED_EDGE('',*,*,#1369,.T.);
#1828=ORIENTED_EDGE('',*,*,#1372,.F.);
#1829=ORIENTED_EDGE('',*,*,#1381,.T.);
#1830=ORIENTED_EDGE('',*,*,#1379,.T.);
#1831=ORIENTED_EDGE('',*,*,#1362,.T.);
#1832=ORIENTED_EDGE('',*,*,#1376,.F.);
#1833=ORIENTED_EDGE('',*,*,#1378,.F.);
#1834=ORIENTED_EDGE('',*,*,#1380,.F.);
#1835=ORIENTED_EDGE('',*,*,#1381,.F.);
#1836=ORIENTED_EDGE('',*,*,#1371,.F.);
#1837=ORIENTED_EDGE('',*,*,#1374,.F.);
#1838=ORIENTED_EDGE('',*,*,#1359,.T.);
#1839=ORIENTED_EDGE('',*,*,#1382,.F.);
#1840=ORIENTED_EDGE('',*,*,#1383,.T.);
#1841=ORIENTED_EDGE('',*,*,#1384,.F.);
#1842=ORIENTED_EDGE('',*,*,#1385,.F.);
#1843=ORIENTED_EDGE('',*,*,#1386,.F.);
#1844=ORIENTED_EDGE('',*,*,#1387,.T.);
#1845=ORIENTED_EDGE('',*,*,#1388,.F.);
#1846=ORIENTED_EDGE('',*,*,#1383,.F.);
#1847=ORIENTED_EDGE('',*,*,#1389,.F.);
#1848=ORIENTED_EDGE('',*,*,#1390,.T.);
#1849=ORIENTED_EDGE('',*,*,#1391,.F.);
#1850=ORIENTED_EDGE('',*,*,#1387,.F.);
#1851=ORIENTED_EDGE('',*,*,#1392,.F.);
#1852=ORIENTED_EDGE('',*,*,#1393,.T.);
#1853=ORIENTED_EDGE('',*,*,#1394,.F.);
#1854=ORIENTED_EDGE('',*,*,#1390,.F.);
#1855=ORIENTED_EDGE('',*,*,#1395,.F.);
#1856=ORIENTED_EDGE('',*,*,#1396,.T.);
#1857=ORIENTED_EDGE('',*,*,#1397,.F.);
#1858=ORIENTED_EDGE('',*,*,#1393,.F.);
#1859=ORIENTED_EDGE('',*,*,#1398,.F.);
#1860=ORIENTED_EDGE('',*,*,#1399,.T.);
#1861=ORIENTED_EDGE('',*,*,#1400,.F.);
#1862=ORIENTED_EDGE('',*,*,#1396,.F.);
#1863=ORIENTED_EDGE('',*,*,#1401,.F.);
#1864=ORIENTED_EDGE('',*,*,#1402,.T.);
#1865=ORIENTED_EDGE('',*,*,#1403,.F.);
#1866=ORIENTED_EDGE('',*,*,#1399,.F.);
#1867=ORIENTED_EDGE('',*,*,#1404,.F.);
#1868=ORIENTED_EDGE('',*,*,#1405,.T.);
#1869=ORIENTED_EDGE('',*,*,#1406,.F.);
#1870=ORIENTED_EDGE('',*,*,#1402,.F.);
#1871=ORIENTED_EDGE('',*,*,#1407,.F.);
#1872=ORIENTED_EDGE('',*,*,#1408,.F.);
#1873=ORIENTED_EDGE('',*,*,#1409,.F.);
#1874=ORIENTED_EDGE('',*,*,#1405,.F.);
#1875=ORIENTED_EDGE('',*,*,#1410,.F.);
#1876=ORIENTED_EDGE('',*,*,#1411,.T.);
#1877=ORIENTED_EDGE('',*,*,#1412,.F.);
#1878=ORIENTED_EDGE('',*,*,#1413,.F.);
#1879=ORIENTED_EDGE('',*,*,#1414,.F.);
#1880=ORIENTED_EDGE('',*,*,#1415,.T.);
#1881=ORIENTED_EDGE('',*,*,#1416,.F.);
#1882=ORIENTED_EDGE('',*,*,#1411,.F.);
#1883=ORIENTED_EDGE('',*,*,#1417,.F.);
#1884=ORIENTED_EDGE('',*,*,#1418,.T.);
#1885=ORIENTED_EDGE('',*,*,#1419,.F.);
#1886=ORIENTED_EDGE('',*,*,#1415,.F.);
#1887=ORIENTED_EDGE('',*,*,#1420,.F.);
#1888=ORIENTED_EDGE('',*,*,#1421,.T.);
#1889=ORIENTED_EDGE('',*,*,#1422,.F.);
#1890=ORIENTED_EDGE('',*,*,#1418,.F.);
#1891=ORIENTED_EDGE('',*,*,#1423,.F.);
#1892=ORIENTED_EDGE('',*,*,#1424,.T.);
#1893=ORIENTED_EDGE('',*,*,#1425,.F.);
#1894=ORIENTED_EDGE('',*,*,#1421,.F.);
#1895=ORIENTED_EDGE('',*,*,#1426,.F.);
#1896=ORIENTED_EDGE('',*,*,#1427,.T.);
#1897=ORIENTED_EDGE('',*,*,#1428,.F.);
#1898=ORIENTED_EDGE('',*,*,#1424,.F.);
#1899=ORIENTED_EDGE('',*,*,#1429,.F.);
#1900=ORIENTED_EDGE('',*,*,#1430,.T.);
#1901=ORIENTED_EDGE('',*,*,#1431,.F.);
#1902=ORIENTED_EDGE('',*,*,#1427,.F.);
#1903=ORIENTED_EDGE('',*,*,#1432,.F.);
#1904=ORIENTED_EDGE('',*,*,#1433,.T.);
#1905=ORIENTED_EDGE('',*,*,#1434,.F.);
#1906=ORIENTED_EDGE('',*,*,#1430,.F.);
#1907=ORIENTED_EDGE('',*,*,#1435,.F.);
#1908=ORIENTED_EDGE('',*,*,#1436,.F.);
#1909=ORIENTED_EDGE('',*,*,#1437,.F.);
#1910=ORIENTED_EDGE('',*,*,#1433,.F.);
#1911=ORIENTED_EDGE('',*,*,#1438,.F.);
#1912=ORIENTED_EDGE('',*,*,#1439,.T.);
#1913=ORIENTED_EDGE('',*,*,#1440,.F.);
#1914=ORIENTED_EDGE('',*,*,#1441,.F.);
#1915=ORIENTED_EDGE('',*,*,#1442,.F.);
#1916=ORIENTED_EDGE('',*,*,#1443,.T.);
#1917=ORIENTED_EDGE('',*,*,#1444,.F.);
#1918=ORIENTED_EDGE('',*,*,#1439,.F.);
#1919=ORIENTED_EDGE('',*,*,#1445,.F.);
#1920=ORIENTED_EDGE('',*,*,#1446,.T.);
#1921=ORIENTED_EDGE('',*,*,#1447,.F.);
#1922=ORIENTED_EDGE('',*,*,#1443,.F.);
#1923=ORIENTED_EDGE('',*,*,#1448,.F.);
#1924=ORIENTED_EDGE('',*,*,#1449,.T.);
#1925=ORIENTED_EDGE('',*,*,#1450,.F.);
#1926=ORIENTED_EDGE('',*,*,#1446,.F.);
#1927=ORIENTED_EDGE('',*,*,#1451,.F.);
#1928=ORIENTED_EDGE('',*,*,#1452,.T.);
#1929=ORIENTED_EDGE('',*,*,#1453,.F.);
#1930=ORIENTED_EDGE('',*,*,#1449,.F.);
#1931=ORIENTED_EDGE('',*,*,#1454,.F.);
#1932=ORIENTED_EDGE('',*,*,#1455,.T.);
#1933=ORIENTED_EDGE('',*,*,#1456,.F.);
#1934=ORIENTED_EDGE('',*,*,#1452,.F.);
#1935=ORIENTED_EDGE('',*,*,#1457,.F.);
#1936=ORIENTED_EDGE('',*,*,#1458,.T.);
#1937=ORIENTED_EDGE('',*,*,#1459,.F.);
#1938=ORIENTED_EDGE('',*,*,#1455,.F.);
#1939=ORIENTED_EDGE('',*,*,#1460,.F.);
#1940=ORIENTED_EDGE('',*,*,#1461,.T.);
#1941=ORIENTED_EDGE('',*,*,#1462,.F.);
#1942=ORIENTED_EDGE('',*,*,#1458,.F.);
#1943=ORIENTED_EDGE('',*,*,#1463,.F.);
#1944=ORIENTED_EDGE('',*,*,#1464,.F.);
#1945=ORIENTED_EDGE('',*,*,#1465,.F.);
#1946=ORIENTED_EDGE('',*,*,#1461,.F.);
#1947=ORIENTED_EDGE('',*,*,#1466,.F.);
#1948=ORIENTED_EDGE('',*,*,#1467,.T.);
#1949=ORIENTED_EDGE('',*,*,#1468,.F.);
#1950=ORIENTED_EDGE('',*,*,#1469,.F.);
#1951=ORIENTED_EDGE('',*,*,#1470,.F.);
#1952=ORIENTED_EDGE('',*,*,#1471,.T.);
#1953=ORIENTED_EDGE('',*,*,#1472,.F.);
#1954=ORIENTED_EDGE('',*,*,#1467,.F.);
#1955=ORIENTED_EDGE('',*,*,#1473,.F.);
#1956=ORIENTED_EDGE('',*,*,#1474,.T.);
#1957=ORIENTED_EDGE('',*,*,#1475,.F.);
#1958=ORIENTED_EDGE('',*,*,#1471,.F.);
#1959=ORIENTED_EDGE('',*,*,#1476,.F.);
#1960=ORIENTED_EDGE('',*,*,#1477,.T.);
#1961=ORIENTED_EDGE('',*,*,#1478,.F.);
#1962=ORIENTED_EDGE('',*,*,#1474,.F.);
#1963=ORIENTED_EDGE('',*,*,#1479,.F.);
#1964=ORIENTED_EDGE('',*,*,#1480,.T.);
#1965=ORIENTED_EDGE('',*,*,#1481,.F.);
#1966=ORIENTED_EDGE('',*,*,#1477,.F.);
#1967=ORIENTED_EDGE('',*,*,#1482,.F.);
#1968=ORIENTED_EDGE('',*,*,#1483,.T.);
#1969=ORIENTED_EDGE('',*,*,#1484,.F.);
#1970=ORIENTED_EDGE('',*,*,#1480,.F.);
#1971=ORIENTED_EDGE('',*,*,#1485,.F.);
#1972=ORIENTED_EDGE('',*,*,#1486,.T.);
#1973=ORIENTED_EDGE('',*,*,#1487,.F.);
#1974=ORIENTED_EDGE('',*,*,#1483,.F.);
#1975=ORIENTED_EDGE('',*,*,#1488,.F.);
#1976=ORIENTED_EDGE('',*,*,#1489,.T.);
#1977=ORIENTED_EDGE('',*,*,#1490,.F.);
#1978=ORIENTED_EDGE('',*,*,#1486,.F.);
#1979=ORIENTED_EDGE('',*,*,#1491,.F.);
#1980=ORIENTED_EDGE('',*,*,#1492,.F.);
#1981=ORIENTED_EDGE('',*,*,#1493,.F.);
#1982=ORIENTED_EDGE('',*,*,#1489,.F.);
#1983=ORIENTED_EDGE('',*,*,#1494,.F.);
#1984=ORIENTED_EDGE('',*,*,#1495,.T.);
#1985=ORIENTED_EDGE('',*,*,#1496,.F.);
#1986=ORIENTED_EDGE('',*,*,#1495,.F.);
#1987=ORIENTED_EDGE('',*,*,#1408,.T.);
#1988=ORIENTED_EDGE('',*,*,#1497,.T.);
#1989=ORIENTED_EDGE('',*,*,#1498,.T.);
#1990=ORIENTED_EDGE('',*,*,#1499,.F.);
#1991=ORIENTED_EDGE('',*,*,#1385,.T.);
#1992=ORIENTED_EDGE('',*,*,#1500,.F.);
#1993=ORIENTED_EDGE('',*,*,#1501,.F.);
#1994=ORIENTED_EDGE('',*,*,#1502,.T.);
#1995=ORIENTED_EDGE('',*,*,#1436,.T.);
#1996=ORIENTED_EDGE('',*,*,#1503,.T.);
#1997=ORIENTED_EDGE('',*,*,#1501,.T.);
#1998=ORIENTED_EDGE('',*,*,#1504,.F.);
#1999=ORIENTED_EDGE('',*,*,#1413,.T.);
#2000=ORIENTED_EDGE('',*,*,#1505,.F.);
#2001=ORIENTED_EDGE('',*,*,#1506,.F.);
#2002=ORIENTED_EDGE('',*,*,#1507,.T.);
#2003=ORIENTED_EDGE('',*,*,#1464,.T.);
#2004=ORIENTED_EDGE('',*,*,#1508,.T.);
#2005=ORIENTED_EDGE('',*,*,#1506,.T.);
#2006=ORIENTED_EDGE('',*,*,#1509,.F.);
#2007=ORIENTED_EDGE('',*,*,#1441,.T.);
#2008=ORIENTED_EDGE('',*,*,#1510,.F.);
#2009=ORIENTED_EDGE('',*,*,#1511,.F.);
#2010=ORIENTED_EDGE('',*,*,#1512,.T.);
#2011=ORIENTED_EDGE('',*,*,#1492,.T.);
#2012=ORIENTED_EDGE('',*,*,#1513,.T.);
#2013=ORIENTED_EDGE('',*,*,#1511,.T.);
#2014=ORIENTED_EDGE('',*,*,#1514,.F.);
#2015=ORIENTED_EDGE('',*,*,#1469,.T.);
#2016=ORIENTED_EDGE('',*,*,#1515,.F.);
#2017=ORIENTED_EDGE('',*,*,#1498,.F.);
#2018=ORIENTED_EDGE('',*,*,#1516,.T.);
#2019=ORIENTED_EDGE('',*,*,#1384,.T.);
#2020=ORIENTED_EDGE('',*,*,#1388,.T.);
#2021=ORIENTED_EDGE('',*,*,#1391,.T.);
#2022=ORIENTED_EDGE('',*,*,#1394,.T.);
#2023=ORIENTED_EDGE('',*,*,#1397,.T.);
#2024=ORIENTED_EDGE('',*,*,#1400,.T.);
#2025=ORIENTED_EDGE('',*,*,#1403,.T.);
#2026=ORIENTED_EDGE('',*,*,#1406,.T.);
#2027=ORIENTED_EDGE('',*,*,#1409,.T.);
#2028=ORIENTED_EDGE('',*,*,#1499,.T.);
#2029=ORIENTED_EDGE('',*,*,#1515,.T.);
#2030=ORIENTED_EDGE('',*,*,#1468,.T.);
#2031=ORIENTED_EDGE('',*,*,#1472,.T.);
#2032=ORIENTED_EDGE('',*,*,#1475,.T.);
#2033=ORIENTED_EDGE('',*,*,#1478,.T.);
#2034=ORIENTED_EDGE('',*,*,#1481,.T.);
#2035=ORIENTED_EDGE('',*,*,#1484,.T.);
#2036=ORIENTED_EDGE('',*,*,#1487,.T.);
#2037=ORIENTED_EDGE('',*,*,#1490,.T.);
#2038=ORIENTED_EDGE('',*,*,#1493,.T.);
#2039=ORIENTED_EDGE('',*,*,#1514,.T.);
#2040=ORIENTED_EDGE('',*,*,#1510,.T.);
#2041=ORIENTED_EDGE('',*,*,#1440,.T.);
#2042=ORIENTED_EDGE('',*,*,#1444,.T.);
#2043=ORIENTED_EDGE('',*,*,#1447,.T.);
#2044=ORIENTED_EDGE('',*,*,#1450,.T.);
#2045=ORIENTED_EDGE('',*,*,#1453,.T.);
#2046=ORIENTED_EDGE('',*,*,#1456,.T.);
#2047=ORIENTED_EDGE('',*,*,#1459,.T.);
#2048=ORIENTED_EDGE('',*,*,#1462,.T.);
#2049=ORIENTED_EDGE('',*,*,#1465,.T.);
#2050=ORIENTED_EDGE('',*,*,#1509,.T.);
#2051=ORIENTED_EDGE('',*,*,#1505,.T.);
#2052=ORIENTED_EDGE('',*,*,#1412,.T.);
#2053=ORIENTED_EDGE('',*,*,#1416,.T.);
#2054=ORIENTED_EDGE('',*,*,#1419,.T.);
#2055=ORIENTED_EDGE('',*,*,#1422,.T.);
#2056=ORIENTED_EDGE('',*,*,#1425,.T.);
#2057=ORIENTED_EDGE('',*,*,#1428,.T.);
#2058=ORIENTED_EDGE('',*,*,#1431,.T.);
#2059=ORIENTED_EDGE('',*,*,#1434,.T.);
#2060=ORIENTED_EDGE('',*,*,#1437,.T.);
#2061=ORIENTED_EDGE('',*,*,#1504,.T.);
#2062=ORIENTED_EDGE('',*,*,#1500,.T.);
#2063=ORIENTED_EDGE('',*,*,#1496,.T.);
#2064=ORIENTED_EDGE('',*,*,#1382,.T.);
#2065=ORIENTED_EDGE('',*,*,#1502,.F.);
#2066=ORIENTED_EDGE('',*,*,#1503,.F.);
#2067=ORIENTED_EDGE('',*,*,#1435,.T.);
#2068=ORIENTED_EDGE('',*,*,#1432,.T.);
#2069=ORIENTED_EDGE('',*,*,#1429,.T.);
#2070=ORIENTED_EDGE('',*,*,#1426,.T.);
#2071=ORIENTED_EDGE('',*,*,#1423,.T.);
#2072=ORIENTED_EDGE('',*,*,#1420,.T.);
#2073=ORIENTED_EDGE('',*,*,#1417,.T.);
#2074=ORIENTED_EDGE('',*,*,#1414,.T.);
#2075=ORIENTED_EDGE('',*,*,#1410,.T.);
#2076=ORIENTED_EDGE('',*,*,#1507,.F.);
#2077=ORIENTED_EDGE('',*,*,#1508,.F.);
#2078=ORIENTED_EDGE('',*,*,#1463,.T.);
#2079=ORIENTED_EDGE('',*,*,#1460,.T.);
#2080=ORIENTED_EDGE('',*,*,#1457,.T.);
#2081=ORIENTED_EDGE('',*,*,#1454,.T.);
#2082=ORIENTED_EDGE('',*,*,#1451,.T.);
#2083=ORIENTED_EDGE('',*,*,#1448,.T.);
#2084=ORIENTED_EDGE('',*,*,#1445,.T.);
#2085=ORIENTED_EDGE('',*,*,#1442,.T.);
#2086=ORIENTED_EDGE('',*,*,#1438,.T.);
#2087=ORIENTED_EDGE('',*,*,#1512,.F.);
#2088=ORIENTED_EDGE('',*,*,#1513,.F.);
#2089=ORIENTED_EDGE('',*,*,#1491,.T.);
#2090=ORIENTED_EDGE('',*,*,#1488,.T.);
#2091=ORIENTED_EDGE('',*,*,#1485,.T.);
#2092=ORIENTED_EDGE('',*,*,#1482,.T.);
#2093=ORIENTED_EDGE('',*,*,#1479,.T.);
#2094=ORIENTED_EDGE('',*,*,#1476,.T.);
#2095=ORIENTED_EDGE('',*,*,#1473,.T.);
#2096=ORIENTED_EDGE('',*,*,#1470,.T.);
#2097=ORIENTED_EDGE('',*,*,#1466,.T.);
#2098=ORIENTED_EDGE('',*,*,#1516,.F.);
#2099=ORIENTED_EDGE('',*,*,#1497,.F.);
#2100=ORIENTED_EDGE('',*,*,#1407,.T.);
#2101=ORIENTED_EDGE('',*,*,#1404,.T.);
#2102=ORIENTED_EDGE('',*,*,#1401,.T.);
#2103=ORIENTED_EDGE('',*,*,#1398,.T.);
#2104=ORIENTED_EDGE('',*,*,#1395,.T.);
#2105=ORIENTED_EDGE('',*,*,#1392,.T.);
#2106=ORIENTED_EDGE('',*,*,#1389,.T.);
#2107=ORIENTED_EDGE('',*,*,#1386,.T.);
#2108=ORIENTED_EDGE('',*,*,#1494,.T.);
#2109=CYLINDRICAL_SURFACE('',#2337,0.34);
#2110=CYLINDRICAL_SURFACE('',#2358,0.25);
#2111=CYLINDRICAL_SURFACE('',#2361,0.33);
#2112=CYLINDRICAL_SURFACE('',#2389,2.);
#2113=CYLINDRICAL_SURFACE('',#2398,2.);
#2114=CYLINDRICAL_SURFACE('',#2412,0.3);
#2115=CYLINDRICAL_SURFACE('',#2416,0.3933);
#2116=CYLINDRICAL_SURFACE('',#2427,0.2942);
#2117=CYLINDRICAL_SURFACE('',#2486,0.21);
#2118=ADVANCED_FACE('',(#218),#2109,.F.);
#2119=ADVANCED_FACE('',(#219),#115,.T.);
#2120=ADVANCED_FACE('',(#220),#116,.T.);
#2121=ADVANCED_FACE('',(#221),#117,.T.);
#2122=ADVANCED_FACE('',(#222),#118,.T.);
#2123=ADVANCED_FACE('',(#223,#100),#119,.T.);
#2124=ADVANCED_FACE('',(#224,#101),#120,.F.);
#2125=ADVANCED_FACE('',(#225),#121,.F.);
#2126=ADVANCED_FACE('',(#226),#122,.F.);
#2127=ADVANCED_FACE('',(#227),#123,.F.);
#2128=ADVANCED_FACE('',(#228),#124,.F.);
#2129=ADVANCED_FACE('',(#229),#125,.T.);
#2130=ADVANCED_FACE('',(#230),#126,.T.);
#2131=ADVANCED_FACE('',(#231),#127,.T.);
#2132=ADVANCED_FACE('',(#232),#128,.T.);
#2133=ADVANCED_FACE('',(#233,#102),#129,.T.);
#2134=ADVANCED_FACE('',(#234,#103),#130,.F.);
#2135=ADVANCED_FACE('',(#235),#2110,.F.);
#2136=ADVANCED_FACE('',(#236),#2111,.F.);
#2137=ADVANCED_FACE('',(#237,#104),#131,.F.);
#2138=ADVANCED_FACE('',(#238,#105),#132,.F.);
#2139=ADVANCED_FACE('',(#239),#133,.T.);
#2140=ADVANCED_FACE('',(#240),#134,.F.);
#2141=ADVANCED_FACE('',(#241),#135,.F.);
#2142=ADVANCED_FACE('',(#242),#136,.F.);
#2143=ADVANCED_FACE('',(#243),#137,.T.);
#2144=ADVANCED_FACE('',(#244),#138,.T.);
#2145=ADVANCED_FACE('',(#245),#139,.F.);
#2146=ADVANCED_FACE('',(#246),#140,.F.);
#2147=ADVANCED_FACE('',(#247),#141,.F.);
#2148=ADVANCED_FACE('',(#248),#142,.F.);
#2149=ADVANCED_FACE('',(#249),#143,.F.);
#2150=ADVANCED_FACE('',(#250),#144,.F.);
#2151=ADVANCED_FACE('',(#251),#145,.F.);
#2152=ADVANCED_FACE('',(#252,#106),#146,.T.);
#2153=ADVANCED_FACE('',(#253,#107),#147,.T.);
#2154=ADVANCED_FACE('',(#254),#148,.T.);
#2155=ADVANCED_FACE('',(#255,#108),#149,.F.);
#2156=ADVANCED_FACE('',(#256),#150,.T.);
#2157=ADVANCED_FACE('',(#257),#63,.T.);
#2158=ADVANCED_FACE('',(#258),#2112,.T.);
#2159=ADVANCED_FACE('',(#259),#151,.T.);
#2160=ADVANCED_FACE('',(#260),#61,.F.);
#2161=ADVANCED_FACE('',(#261),#152,.T.);
#2162=ADVANCED_FACE('',(#262),#2113,.T.);
#2163=ADVANCED_FACE('',(#263),#64,.T.);
#2164=ADVANCED_FACE('',(#264,#109),#153,.T.);
#2165=ADVANCED_FACE('',(#265,#110),#154,.T.);
#2166=ADVANCED_FACE('',(#266),#155,.T.);
#2167=ADVANCED_FACE('',(#267),#156,.T.);
#2168=ADVANCED_FACE('',(#268),#157,.T.);
#2169=ADVANCED_FACE('',(#269),#158,.T.);
#2170=ADVANCED_FACE('',(#270),#159,.T.);
#2171=ADVANCED_FACE('',(#271),#160,.T.);
#2172=ADVANCED_FACE('',(#272),#2114,.T.);
#2173=ADVANCED_FACE('',(#273,#111),#161,.T.);
#2174=ADVANCED_FACE('',(#274),#2115,.T.);
#2175=ADVANCED_FACE('',(#275),#65,.T.);
#2176=ADVANCED_FACE('',(#276),#162,.T.);
#2177=ADVANCED_FACE('',(#277),#62,.T.);
#2178=ADVANCED_FACE('',(#278),#2116,.T.);
#2179=ADVANCED_FACE('',(#279),#66,.T.);
#2180=ADVANCED_FACE('',(#280),#163,.T.);
#2181=ADVANCED_FACE('',(#281),#67,.T.);
#2182=ADVANCED_FACE('',(#282),#164,.T.);
#2183=ADVANCED_FACE('',(#283),#165,.T.);
#2184=ADVANCED_FACE('',(#284),#166,.T.);
#2185=ADVANCED_FACE('',(#285),#167,.T.);
#2186=ADVANCED_FACE('',(#286),#168,.T.);
#2187=ADVANCED_FACE('',(#287),#169,.T.);
#2188=ADVANCED_FACE('',(#288),#170,.T.);
#2189=ADVANCED_FACE('',(#289,#112),#171,.F.);
#2190=ADVANCED_FACE('',(#290),#172,.F.);
#2191=ADVANCED_FACE('',(#291),#173,.F.);
#2192=ADVANCED_FACE('',(#292),#174,.F.);
#2193=ADVANCED_FACE('',(#293),#175,.F.);
#2194=ADVANCED_FACE('',(#294),#176,.F.);
#2195=ADVANCED_FACE('',(#295),#177,.F.);
#2196=ADVANCED_FACE('',(#296),#178,.F.);
#2197=ADVANCED_FACE('',(#297),#179,.F.);
#2198=ADVANCED_FACE('',(#298),#180,.F.);
#2199=ADVANCED_FACE('',(#299),#181,.F.);
#2200=ADVANCED_FACE('',(#300),#182,.F.);
#2201=ADVANCED_FACE('',(#301),#183,.F.);
#2202=ADVANCED_FACE('',(#302),#184,.F.);
#2203=ADVANCED_FACE('',(#303),#185,.F.);
#2204=ADVANCED_FACE('',(#304),#186,.F.);
#2205=ADVANCED_FACE('',(#305),#187,.F.);
#2206=ADVANCED_FACE('',(#306),#188,.F.);
#2207=ADVANCED_FACE('',(#307),#189,.F.);
#2208=ADVANCED_FACE('',(#308),#190,.F.);
#2209=ADVANCED_FACE('',(#309),#191,.F.);
#2210=ADVANCED_FACE('',(#310),#192,.F.);
#2211=ADVANCED_FACE('',(#311),#193,.F.);
#2212=ADVANCED_FACE('',(#312),#194,.F.);
#2213=ADVANCED_FACE('',(#313),#195,.F.);
#2214=ADVANCED_FACE('',(#314),#196,.F.);
#2215=ADVANCED_FACE('',(#315),#197,.F.);
#2216=ADVANCED_FACE('',(#316),#198,.F.);
#2217=ADVANCED_FACE('',(#317),#199,.F.);
#2218=ADVANCED_FACE('',(#318),#200,.F.);
#2219=ADVANCED_FACE('',(#319),#201,.F.);
#2220=ADVANCED_FACE('',(#320),#202,.F.);
#2221=ADVANCED_FACE('',(#321),#203,.F.);
#2222=ADVANCED_FACE('',(#322),#204,.F.);
#2223=ADVANCED_FACE('',(#323),#205,.F.);
#2224=ADVANCED_FACE('',(#324),#206,.F.);
#2225=ADVANCED_FACE('',(#325),#207,.F.);
#2226=ADVANCED_FACE('',(#326),#2117,.F.);
#2227=ADVANCED_FACE('',(#327),#208,.T.);
#2228=ADVANCED_FACE('',(#328),#209,.T.);
#2229=ADVANCED_FACE('',(#329),#210,.T.);
#2230=ADVANCED_FACE('',(#330),#211,.T.);
#2231=ADVANCED_FACE('',(#331),#212,.T.);
#2232=ADVANCED_FACE('',(#332),#213,.T.);
#2233=ADVANCED_FACE('',(#333),#214,.T.);
#2234=ADVANCED_FACE('',(#334),#215,.T.);
#2235=ADVANCED_FACE('',(#335,#113),#216,.T.);
#2236=ADVANCED_FACE('',(#336,#114),#217,.F.);
#2237=CLOSED_SHELL('',(#2118,#2119,#2120,#2121,#2122,#2123,#2124));
#2238=CLOSED_SHELL('',(#2125,#2126,#2127,#2128,#2129,#2130,#2131,#2132,
#2133,#2134));
#2239=CLOSED_SHELL('',(#2135,#2136,#2137,#2138,#2139,#2140,#2141,#2142,
#2143,#2144,#2145,#2146,#2147,#2148,#2149,#2150,#2151,#2152,#2153,#2154,
#2155));
#2240=CLOSED_SHELL('',(#2156,#2157,#2158,#2159));
#2241=CLOSED_SHELL('',(#2160,#2161,#2162,#2163,#2164));
#2242=CLOSED_SHELL('',(#2165,#2166,#2167,#2168,#2169,#2170,#2171,#2172,
#2173,#2174,#2175,#2176,#2177));
#2243=CLOSED_SHELL('',(#2178,#2179,#2180,#2181,#2182,#2183,#2184,#2185,
#2186,#2187,#2188,#2189));
#2244=CLOSED_SHELL('',(#2190,#2191,#2192,#2193,#2194,#2195,#2196,#2197,
#2198,#2199,#2200,#2201,#2202,#2203,#2204,#2205,#2206,#2207,#2208,#2209,
#2210,#2211,#2212,#2213,#2214,#2215,#2216,#2217,#2218,#2219,#2220,#2221,
#2222,#2223,#2224,#2225,#2226,#2227,#2228,#2229,#2230,#2231,#2232,#2233,
#2234,#2235,#2236));
#2245=DERIVED_UNIT_ELEMENT(#2261,1.);
#2246=DERIVED_UNIT_ELEMENT(#3775,-3.);
#2247=DERIVED_UNIT_ELEMENT(#2261,1.);
#2248=DERIVED_UNIT_ELEMENT(#3775,-3.);
#2249=DERIVED_UNIT_ELEMENT(#2261,1.);
#2250=DERIVED_UNIT_ELEMENT(#3775,-3.);
#2251=DERIVED_UNIT_ELEMENT(#2261,1.);
#2252=DERIVED_UNIT_ELEMENT(#3775,-3.);
#2253=DERIVED_UNIT_ELEMENT(#2261,1.);
#2254=DERIVED_UNIT_ELEMENT(#3775,-3.);
#2255=DERIVED_UNIT_ELEMENT(#2261,1.);
#2256=DERIVED_UNIT_ELEMENT(#3775,-3.);
#2257=DERIVED_UNIT_ELEMENT(#2261,1.);
#2258=DERIVED_UNIT_ELEMENT(#3775,-3.);
#2259=DERIVED_UNIT_ELEMENT(#2261,1.);
#2260=DERIVED_UNIT_ELEMENT(#3775,-3.);
#2261=(
MASS_UNIT()
NAMED_UNIT(*)
SI_UNIT(.KILO.,.GRAM.)
);
#2262=DERIVED_UNIT((#2245,#2246));
#2263=DERIVED_UNIT((#2247,#2248));
#2264=DERIVED_UNIT((#2249,#2250));
#2265=DERIVED_UNIT((#2251,#2252));
#2266=DERIVED_UNIT((#2253,#2254));
#2267=DERIVED_UNIT((#2255,#2256));
#2268=DERIVED_UNIT((#2257,#2258));
#2269=DERIVED_UNIT((#2259,#2260));
#2270=MEASURE_REPRESENTATION_ITEM('density measure',
POSITIVE_RATIO_MEASURE(7850.),#2262);
#2271=MEASURE_REPRESENTATION_ITEM('density measure',
POSITIVE_RATIO_MEASURE(7850.),#2263);
#2272=MEASURE_REPRESENTATION_ITEM('density measure',
POSITIVE_RATIO_MEASURE(7850.),#2264);
#2273=MEASURE_REPRESENTATION_ITEM('density measure',
POSITIVE_RATIO_MEASURE(7850.),#2265);
#2274=MEASURE_REPRESENTATION_ITEM('density measure',
POSITIVE_RATIO_MEASURE(7850.),#2266);
#2275=MEASURE_REPRESENTATION_ITEM('density measure',
POSITIVE_RATIO_MEASURE(7850.),#2267);
#2276=MEASURE_REPRESENTATION_ITEM('density measure',
POSITIVE_RATIO_MEASURE(7850.),#2268);
#2277=MEASURE_REPRESENTATION_ITEM('density measure',
POSITIVE_RATIO_MEASURE(7850.),#2269);
#2278=PROPERTY_DEFINITION_REPRESENTATION(#2318,#2294);
#2279=PROPERTY_DEFINITION_REPRESENTATION(#2319,#2295);
#2280=PROPERTY_DEFINITION_REPRESENTATION(#2320,#2296);
#2281=PROPERTY_DEFINITION_REPRESENTATION(#2321,#2297);
#2282=PROPERTY_DEFINITION_REPRESENTATION(#2322,#2298);
#2283=PROPERTY_DEFINITION_REPRESENTATION(#2323,#2299);
#2284=PROPERTY_DEFINITION_REPRESENTATION(#2324,#2300);
#2285=PROPERTY_DEFINITION_REPRESENTATION(#2325,#2301);
#2286=PROPERTY_DEFINITION_REPRESENTATION(#2326,#2302);
#2287=PROPERTY_DEFINITION_REPRESENTATION(#2327,#2303);
#2288=PROPERTY_DEFINITION_REPRESENTATION(#2328,#2304);
#2289=PROPERTY_DEFINITION_REPRESENTATION(#2329,#2305);
#2290=PROPERTY_DEFINITION_REPRESENTATION(#2330,#2306);
#2291=PROPERTY_DEFINITION_REPRESENTATION(#2331,#2307);
#2292=PROPERTY_DEFINITION_REPRESENTATION(#2332,#2308);
#2293=PROPERTY_DEFINITION_REPRESENTATION(#2333,#2309);
#2294=REPRESENTATION('material name',(#2310),#3763);
#2295=REPRESENTATION('density',(#2270),#3763);
#2296=REPRESENTATION('material name',(#2311),#3764);
#2297=REPRESENTATION('density',(#2271),#3764);
#2298=REPRESENTATION('material name',(#2312),#3765);
#2299=REPRESENTATION('density',(#2272),#3765);
#2300=REPRESENTATION('material name',(#2313),#3767);
#2301=REPRESENTATION('density',(#2273),#3767);
#2302=REPRESENTATION('material name',(#2314),#3768);
#2303=REPRESENTATION('density',(#2274),#3768);
#2304=REPRESENTATION('material name',(#2315),#3769);
#2305=REPRESENTATION('density',(#2275),#3769);
#2306=REPRESENTATION('material name',(#2316),#3770);
#2307=REPRESENTATION('density',(#2276),#3770);
#2308=REPRESENTATION('material name',(#2317),#3772);
#2309=REPRESENTATION('density',(#2277),#3772);
#2310=DESCRIPTIVE_REPRESENTATION_ITEM('Steel','Steel');
#2311=DESCRIPTIVE_REPRESENTATION_ITEM('Steel','Steel');
#2312=DESCRIPTIVE_REPRESENTATION_ITEM('Steel','Steel');
#2313=DESCRIPTIVE_REPRESENTATION_ITEM('Steel','Steel');
#2314=DESCRIPTIVE_REPRESENTATION_ITEM('Steel','Steel');
#2315=DESCRIPTIVE_REPRESENTATION_ITEM('Steel','Steel');
#2316=DESCRIPTIVE_REPRESENTATION_ITEM('Steel','Steel');
#2317=DESCRIPTIVE_REPRESENTATION_ITEM('Steel','Steel');
#2318=PROPERTY_DEFINITION('material property','material name',#3828);
#2319=PROPERTY_DEFINITION('material property','density of part',#3828);
#2320=PROPERTY_DEFINITION('material property','material name',#3829);
#2321=PROPERTY_DEFINITION('material property','density of part',#3829);
#2322=PROPERTY_DEFINITION('material property','material name',#3830);
#2323=PROPERTY_DEFINITION('material property','density of part',#3830);
#2324=PROPERTY_DEFINITION('material property','material name',#3832);
#2325=PROPERTY_DEFINITION('material property','density of part',#3832);
#2326=PROPERTY_DEFINITION('material property','material name',#3833);
#2327=PROPERTY_DEFINITION('material property','density of part',#3833);
#2328=PROPERTY_DEFINITION('material property','material name',#3834);
#2329=PROPERTY_DEFINITION('material property','density of part',#3834);
#2330=PROPERTY_DEFINITION('material property','material name',#3835);
#2331=PROPERTY_DEFINITION('material property','density of part',#3835);
#2332=PROPERTY_DEFINITION('material property','material name',#3837);
#2333=PROPERTY_DEFINITION('material property','density of part',#3837);
#2334=AXIS2_PLACEMENT_3D('',#3102,#2502,#2503);
#2335=AXIS2_PLACEMENT_3D('',#3103,#2504,#2505);
#2336=AXIS2_PLACEMENT_3D('',#3104,#2506,#2507);
#2337=AXIS2_PLACEMENT_3D('',#3105,#2508,#2509);
#2338=AXIS2_PLACEMENT_3D('',#3107,#2510,#2511);
#2339=AXIS2_PLACEMENT_3D('',#3110,#2513,#2514);
#2340=AXIS2_PLACEMENT_3D('',#3111,#2515,#2516);
#2341=AXIS2_PLACEMENT_3D('',#3120,#2521,#2522);
#2342=AXIS2_PLACEMENT_3D('',#3126,#2526,#2527);
#2343=AXIS2_PLACEMENT_3D('',#3132,#2531,#2532);
#2344=AXIS2_PLACEMENT_3D('',#3135,#2535,#2536);
#2345=AXIS2_PLACEMENT_3D('',#3136,#2537,#2538);
#2346=AXIS2_PLACEMENT_3D('',#3137,#2539,#2540);
#2347=AXIS2_PLACEMENT_3D('',#3138,#2541,#2542);
#2348=AXIS2_PLACEMENT_3D('',#3147,#2547,#2548);
#2349=AXIS2_PLACEMENT_3D('',#3153,#2552,#2553);
#2350=AXIS2_PLACEMENT_3D('',#3159,#2557,#2558);
#2351=AXIS2_PLACEMENT_3D('',#3162,#2561,#2562);
#2352=AXIS2_PLACEMENT_3D('',#3171,#2567,#2568);
#2353=AXIS2_PLACEMENT_3D('',#3177,#2572,#2573);
#2354=AXIS2_PLACEMENT_3D('',#3183,#2577,#2578);
#2355=AXIS2_PLACEMENT_3D('',#3186,#2581,#2582);
#2356=AXIS2_PLACEMENT_3D('',#3187,#2583,#2584);
#2357=AXIS2_PLACEMENT_3D('',#3188,#2585,#2586);
#2358=AXIS2_PLACEMENT_3D('',#3189,#2587,#2588);
#2359=AXIS2_PLACEMENT_3D('',#3191,#2589,#2590);
#2360=AXIS2_PLACEMENT_3D('',#3194,#2592,#2593);
#2361=AXIS2_PLACEMENT_3D('',#3195,#2594,#2595);
#2362=AXIS2_PLACEMENT_3D('',#3197,#2596,#2597);
#2363=AXIS2_PLACEMENT_3D('',#3200,#2599,#2600);
#2364=AXIS2_PLACEMENT_3D('',#3201,#2601,#2602);
#2365=AXIS2_PLACEMENT_3D('',#3212,#2608,#2609);
#2366=AXIS2_PLACEMENT_3D('',#3223,#2615,#2616);
#2367=AXIS2_PLACEMENT_3D('',#3226,#2619,#2620);
#2368=AXIS2_PLACEMENT_3D('',#3245,#2631,#2632);
#2369=AXIS2_PLACEMENT_3D('',#3249,#2635,#2636);
#2370=AXIS2_PLACEMENT_3D('',#3253,#2639,#2640);
#2371=AXIS2_PLACEMENT_3D('',#3263,#2646,#2647);
#2372=AXIS2_PLACEMENT_3D('',#3274,#2654,#2655);
#2373=AXIS2_PLACEMENT_3D('',#3276,#2657,#2658);
#2374=AXIS2_PLACEMENT_3D('',#3278,#2660,#2661);
#2375=AXIS2_PLACEMENT_3D('',#3279,#2662,#2663);
#2376=AXIS2_PLACEMENT_3D('',#3285,#2667,#2668);
#2377=AXIS2_PLACEMENT_3D('',#3289,#2671,#2672);
#2378=AXIS2_PLACEMENT_3D('',#3293,#2675,#2676);
#2379=AXIS2_PLACEMENT_3D('',#3295,#2678,#2679);
#2380=AXIS2_PLACEMENT_3D('',#3299,#2682,#2683);
#2381=AXIS2_PLACEMENT_3D('',#3303,#2686,#2687);
#2382=AXIS2_PLACEMENT_3D('',#3305,#2689,#2690);
#2383=AXIS2_PLACEMENT_3D('',#3306,#2691,#2692);
#2384=AXIS2_PLACEMENT_3D('',#3307,#2693,#2694);
#2385=AXIS2_PLACEMENT_3D('',#3308,#2695,#2696);
#2386=AXIS2_PLACEMENT_3D('',#3310,#2697,#2698);
#2387=AXIS2_PLACEMENT_3D('',#3311,#2699,#2700);
#2388=AXIS2_PLACEMENT_3D('',#3313,#2701,#2702);
#2389=AXIS2_PLACEMENT_3D('',#3315,#2704,#2705);
#2390=AXIS2_PLACEMENT_3D('',#3317,#2706,#2707);
#2391=AXIS2_PLACEMENT_3D('',#3319,#2709,#2710);
#2392=AXIS2_PLACEMENT_3D('',#3320,#2711,#2712);
#2393=AXIS2_PLACEMENT_3D('',#3321,#2713,#2714);
#2394=AXIS2_PLACEMENT_3D('',#3323,#2715,#2716);
#2395=AXIS2_PLACEMENT_3D('',#3325,#2717,#2718);
#2396=AXIS2_PLACEMENT_3D('',#3326,#2719,#2720);
#2397=AXIS2_PLACEMENT_3D('',#3328,#2721,#2722);
#2398=AXIS2_PLACEMENT_3D('',#3329,#2723,#2724);
#2399=AXIS2_PLACEMENT_3D('',#3331,#2725,#2726);
#2400=AXIS2_PLACEMENT_3D('',#3333,#2728,#2729);
#2401=AXIS2_PLACEMENT_3D('',#3335,#2730,#2731);
#2402=AXIS2_PLACEMENT_3D('',#3337,#2733,#2734);
#2403=AXIS2_PLACEMENT_3D('',#3338,#2735,#2736);
#2404=AXIS2_PLACEMENT_3D('',#3339,#2737,#2738);
#2405=AXIS2_PLACEMENT_3D('',#3353,#2745,#2746);
#2406=AXIS2_PLACEMENT_3D('',#3354,#2747,#2748);
#2407=AXIS2_PLACEMENT_3D('',#3360,#2752,#2753);
#2408=AXIS2_PLACEMENT_3D('',#3364,#2756,#2757);
#2409=AXIS2_PLACEMENT_3D('',#3368,#2760,#2761);
#2410=AXIS2_PLACEMENT_3D('',#3372,#2764,#2765);
#2411=AXIS2_PLACEMENT_3D('',#3376,#2768,#2769);
#2412=AXIS2_PLACEMENT_3D('',#3378,#2771,#2772);
#2413=AXIS2_PLACEMENT_3D('',#3380,#2773,#2774);
#2414=AXIS2_PLACEMENT_3D('',#3383,#2776,#2777);
#2415=AXIS2_PLACEMENT_3D('',#3384,#2778,#2779);
#2416=AXIS2_PLACEMENT_3D('',#3385,#2780,#2781);
#2417=AXIS2_PLACEMENT_3D('',#3387,#2782,#2783);
#2418=AXIS2_PLACEMENT_3D('',#3389,#2785,#2786);
#2419=AXIS2_PLACEMENT_3D('',#3391,#2787,#2788);
#2420=AXIS2_PLACEMENT_3D('',#3393,#2790,#2791);
#2421=AXIS2_PLACEMENT_3D('',#3394,#2792,#2793);
#2422=AXIS2_PLACEMENT_3D('',#3396,#2794,#2795);
#2423=AXIS2_PLACEMENT_3D('',#3397,#2796,#2797);
#2424=AXIS2_PLACEMENT_3D('',#3398,#2798,#2799);
#2425=AXIS2_PLACEMENT_3D('',#3399,#2800,#2801);
#2426=AXIS2_PLACEMENT_3D('',#3400,#2802,#2803);
#2427=AXIS2_PLACEMENT_3D('',#3401,#2804,#2805);
#2428=AXIS2_PLACEMENT_3D('',#3403,#2806,#2807);
#2429=AXIS2_PLACEMENT_3D('',#3406,#2809,#2810);
#2430=AXIS2_PLACEMENT_3D('',#3407,#2811,#2812);
#2431=AXIS2_PLACEMENT_3D('',#3409,#2813,#2814);
#2432=AXIS2_PLACEMENT_3D('',#3411,#2816,#2817);
#2433=AXIS2_PLACEMENT_3D('',#3412,#2818,#2819);
#2434=AXIS2_PLACEMENT_3D('',#3414,#2820,#2821);
#2435=AXIS2_PLACEMENT_3D('',#3440,#2823,#2824);
#2436=AXIS2_PLACEMENT_3D('',#3446,#2828,#2829);
#2437=AXIS2_PLACEMENT_3D('',#3450,#2832,#2833);
#2438=AXIS2_PLACEMENT_3D('',#3454,#2836,#2837);
#2439=AXIS2_PLACEMENT_3D('',#3458,#2840,#2841);
#2440=AXIS2_PLACEMENT_3D('',#3462,#2844,#2845);
#2441=AXIS2_PLACEMENT_3D('',#3464,#2847,#2848);
#2442=AXIS2_PLACEMENT_3D('',#3465,#2849,#2850);
#2443=AXIS2_PLACEMENT_3D('',#3466,#2851,#2852);
#2444=AXIS2_PLACEMENT_3D('',#3467,#2853,#2854);
#2445=AXIS2_PLACEMENT_3D('',#3468,#2855,#2856);
#2446=AXIS2_PLACEMENT_3D('',#3469,#2857,#2858);
#2447=AXIS2_PLACEMENT_3D('',#3470,#2859,#2860);
#2448=AXIS2_PLACEMENT_3D('',#3471,#2861,#2862);
#2449=AXIS2_PLACEMENT_3D('',#3472,#2863,#2864);
#2450=AXIS2_PLACEMENT_3D('',#3473,#2865,#2866);
#2451=AXIS2_PLACEMENT_3D('',#3482,#2871,#2872);
#2452=AXIS2_PLACEMENT_3D('',#3488,#2876,#2877);
#2453=AXIS2_PLACEMENT_3D('',#3494,#2881,#2882);
#2454=AXIS2_PLACEMENT_3D('',#3500,#2886,#2887);
#2455=AXIS2_PLACEMENT_3D('',#3506,#2891,#2892);
#2456=AXIS2_PLACEMENT_3D('',#3512,#2896,#2897);
#2457=AXIS2_PLACEMENT_3D('',#3518,#2901,#2902);
#2458=AXIS2_PLACEMENT_3D('',#3524,#2906,#2907);
#2459=AXIS2_PLACEMENT_3D('',#3530,#2911,#2912);
#2460=AXIS2_PLACEMENT_3D('',#3539,#2917,#2918);
#2461=AXIS2_PLACEMENT_3D('',#3545,#2922,#2923);
#2462=AXIS2_PLACEMENT_3D('',#3551,#2927,#2928);
#2463=AXIS2_PLACEMENT_3D('',#3557,#2932,#2933);
#2464=AXIS2_PLACEMENT_3D('',#3563,#2937,#2938);
#2465=AXIS2_PLACEMENT_3D('',#3569,#2942,#2943);
#2466=AXIS2_PLACEMENT_3D('',#3575,#2947,#2948);
#2467=AXIS2_PLACEMENT_3D('',#3581,#2952,#2953);
#2468=AXIS2_PLACEMENT_3D('',#3587,#2957,#2958);
#2469=AXIS2_PLACEMENT_3D('',#3596,#2963,#2964);
#2470=AXIS2_PLACEMENT_3D('',#3602,#2968,#2969);
#2471=AXIS2_PLACEMENT_3D('',#3608,#2973,#2974);
#2472=AXIS2_PLACEMENT_3D('',#3614,#2978,#2979);
#2473=AXIS2_PLACEMENT_3D('',#3620,#2983,#2984);
#2474=AXIS2_PLACEMENT_3D('',#3626,#2988,#2989);
#2475=AXIS2_PLACEMENT_3D('',#3632,#2993,#2994);
#2476=AXIS2_PLACEMENT_3D('',#3638,#2998,#2999);
#2477=AXIS2_PLACEMENT_3D('',#3644,#3003,#3004);
#2478=AXIS2_PLACEMENT_3D('',#3653,#3009,#3010);
#2479=AXIS2_PLACEMENT_3D('',#3659,#3014,#3015);
#2480=AXIS2_PLACEMENT_3D('',#3665,#3019,#3020);
#2481=AXIS2_PLACEMENT_3D('',#3671,#3024,#3025);
#2482=AXIS2_PLACEMENT_3D('',#3677,#3029,#3030);
#2483=AXIS2_PLACEMENT_3D('',#3683,#3034,#3035);
#2484=AXIS2_PLACEMENT_3D('',#3689,#3039,#3040);
#2485=AXIS2_PLACEMENT_3D('',#3695,#3044,#3045);
#2486=AXIS2_PLACEMENT_3D('',#3701,#3049,#3050);
#2487=AXIS2_PLACEMENT_3D('',#3703,#3051,#3052);
#2488=AXIS2_PLACEMENT_3D('',#3706,#3054,#3055);
#2489=AXIS2_PLACEMENT_3D('',#3707,#3056,#3057);
#2490=AXIS2_PLACEMENT_3D('',#3713,#3061,#3062);
#2491=AXIS2_PLACEMENT_3D('',#3719,#3066,#3067);
#2492=AXIS2_PLACEMENT_3D('',#3722,#3070,#3071);
#2493=AXIS2_PLACEMENT_3D('',#3728,#3075,#3076);
#2494=AXIS2_PLACEMENT_3D('',#3731,#3079,#3080);
#2495=AXIS2_PLACEMENT_3D('',#3737,#3084,#3085);
#2496=AXIS2_PLACEMENT_3D('',#3740,#3088,#3089);
#2497=AXIS2_PLACEMENT_3D('',#3743,#3092,#3093);
#2498=AXIS2_PLACEMENT_3D('',#3744,#3094,#3095);
#2499=AXIS2_PLACEMENT_3D('',#3745,#3096,#3097);
#2500=AXIS2_PLACEMENT_3D('',#3746,#3098,#3099);
#2501=AXIS2_PLACEMENT_3D('',#3747,#3100,#3101);
#2502=DIRECTION('axis',(0.,0.,1.));
#2503=DIRECTION('refdir',(1.,0.,0.));
#2504=DIRECTION('axis',(0.,0.,1.));
#2505=DIRECTION('refdir',(1.,0.,0.));
#2506=DIRECTION('axis',(0.,0.,1.));
#2507=DIRECTION('refdir',(1.,0.,0.));
#2508=DIRECTION('center_axis',(0.,0.,1.));
#2509=DIRECTION('ref_axis',(1.,0.,0.));
#2510=DIRECTION('center_axis',(0.,0.,1.));
#2511=DIRECTION('ref_axis',(1.,0.,0.));
#2512=DIRECTION('',(0.,0.,1.));
#2513=DIRECTION('center_axis',(0.,0.,-1.));
#2514=DIRECTION('ref_axis',(1.,0.,0.));
#2515=DIRECTION('center_axis',(0.,1.,0.));
#2516=DIRECTION('ref_axis',(-1.,0.,0.));
#2517=DIRECTION('',(-1.,0.,0.));
#2518=DIRECTION('',(0.,0.,1.));
#2519=DIRECTION('',(-1.,0.,0.));
#2520=DIRECTION('',(0.,0.,1.));
#2521=DIRECTION('center_axis',(1.,0.,0.));
#2522=DIRECTION('ref_axis',(0.,1.,0.));
#2523=DIRECTION('',(0.,1.,0.));
#2524=DIRECTION('',(0.,1.,0.));
#2525=DIRECTION('',(0.,0.,1.));
#2526=DIRECTION('center_axis',(0.,-1.,0.));
#2527=DIRECTION('ref_axis',(1.,0.,0.));
#2528=DIRECTION('',(1.,0.,0.));
#2529=DIRECTION('',(1.,0.,0.));
#2530=DIRECTION('',(0.,0.,1.));
#2531=DIRECTION('center_axis',(-1.,0.,0.));
#2532=DIRECTION('ref_axis',(0.,-1.,0.));
#2533=DIRECTION('',(0.,-1.,0.));
#2534=DIRECTION('',(0.,-1.,0.));
#2535=DIRECTION('center_axis',(0.,0.,1.));
#2536=DIRECTION('ref_axis',(1.,0.,0.));
#2537=DIRECTION('center_axis',(0.,0.,1.));
#2538=DIRECTION('ref_axis',(1.,0.,0.));
#2539=DIRECTION('axis',(0.,0.,1.));
#2540=DIRECTION('refdir',(1.,0.,0.));
#2541=DIRECTION('center_axis',(0.,-1.,0.));
#2542=DIRECTION('ref_axis',(1.,0.,0.));
#2543=DIRECTION('',(-1.,0.,0.));
#2544=DIRECTION('',(0.,0.,1.));
#2545=DIRECTION('',(1.,0.,0.));
#2546=DIRECTION('',(0.,0.,1.));
#2547=DIRECTION('center_axis',(-1.,0.,0.));
#2548=DIRECTION('ref_axis',(0.,-1.,0.));
#2549=DIRECTION('',(0.,1.,0.));
#2550=DIRECTION('',(0.,-1.,0.));
#2551=DIRECTION('',(0.,0.,1.));
#2552=DIRECTION('center_axis',(0.,1.,0.));
#2553=DIRECTION('ref_axis',(-1.,0.,0.));
#2554=DIRECTION('',(1.,0.,0.));
#2555=DIRECTION('',(-1.,0.,0.));
#2556=DIRECTION('',(0.,0.,1.));
#2557=DIRECTION('center_axis',(1.,0.,0.));
#2558=DIRECTION('ref_axis',(0.,1.,0.));
#2559=DIRECTION('',(0.,-1.,0.));
#2560=DIRECTION('',(0.,1.,0.));
#2561=DIRECTION('center_axis',(0.,1.,0.));
#2562=DIRECTION('ref_axis',(-1.,0.,0.));
#2563=DIRECTION('',(-1.,0.,0.));
#2564=DIRECTION('',(0.,0.,1.));
#2565=DIRECTION('',(-1.,0.,0.));
#2566=DIRECTION('',(0.,0.,1.));
#2567=DIRECTION('center_axis',(1.,0.,0.));
#2568=DIRECTION('ref_axis',(0.,1.,0.));
#2569=DIRECTION('',(0.,1.,0.));
#2570=DIRECTION('',(0.,1.,0.));
#2571=DIRECTION('',(0.,0.,1.));
#2572=DIRECTION('center_axis',(0.,-1.,0.));
#2573=DIRECTION('ref_axis',(1.,0.,0.));
#2574=DIRECTION('',(1.,0.,0.));
#2575=DIRECTION('',(1.,0.,0.));
#2576=DIRECTION('',(0.,0.,1.));
#2577=DIRECTION('center_axis',(-1.,0.,0.));
#2578=DIRECTION('ref_axis',(0.,-1.,0.));
#2579=DIRECTION('',(0.,-1.,0.));
#2580=DIRECTION('',(0.,-1.,0.));
#2581=DIRECTION('center_axis',(0.,0.,1.));
#2582=DIRECTION('ref_axis',(1.,0.,0.));
#2583=DIRECTION('center_axis',(0.,0.,1.));
#2584=DIRECTION('ref_axis',(1.,0.,0.));
#2585=DIRECTION('axis',(0.,0.,1.));
#2586=DIRECTION('refdir',(1.,0.,0.));
#2587=DIRECTION('center_axis',(0.,1.,0.));
#2588=DIRECTION('ref_axis',(1.,0.,0.));
#2589=DIRECTION('center_axis',(0.,1.,0.));
#2590=DIRECTION('ref_axis',(1.,0.,0.));
#2591=DIRECTION('',(0.,1.,0.));
#2592=DIRECTION('center_axis',(0.,-1.,0.));
#2593=DIRECTION('ref_axis',(1.,0.,0.));
#2594=DIRECTION('center_axis',(0.,1.,0.));
#2595=DIRECTION('ref_axis',(1.,0.,0.));
#2596=DIRECTION('center_axis',(0.,1.,0.));
#2597=DIRECTION('ref_axis',(1.,0.,0.));
#2598=DIRECTION('',(0.,1.,0.));
#2599=DIRECTION('center_axis',(0.,-1.,0.));
#2600=DIRECTION('ref_axis',(1.,0.,0.));
#2601=DIRECTION('center_axis',(0.,1.,0.));
#2602=DIRECTION('ref_axis',(-1.,0.,0.));
#2603=DIRECTION('',(0.,0.,1.));
#2604=DIRECTION('',(-1.,0.,0.));
#2605=DIRECTION('',(-1.,0.,0.));
#2606=DIRECTION('',(0.,0.,-1.));
#2607=DIRECTION('',(1.,0.,0.));
#2608=DIRECTION('center_axis',(0.,-1.,0.));
#2609=DIRECTION('ref_axis',(1.,0.,0.));
#2610=DIRECTION('',(0.,0.,-1.));
#2611=DIRECTION('',(-1.,0.,0.));
#2612=DIRECTION('',(0.,0.,1.));
#2613=DIRECTION('',(1.,0.,0.));
#2614=DIRECTION('',(1.,0.,0.));
#2615=DIRECTION('center_axis',(0.,0.,1.));
#2616=DIRECTION('ref_axis',(1.,0.,0.));
#2617=DIRECTION('',(0.,1.,0.));
#2618=DIRECTION('',(0.,-1.,0.));
#2619=DIRECTION('center_axis',(0.,0.,1.));
#2620=DIRECTION('ref_axis',(1.,0.,0.));
#2621=DIRECTION('',(0.,1.,0.));
#2622=DIRECTION('',(-1.,0.,0.));
#2623=DIRECTION('',(0.,-1.,0.));
#2624=DIRECTION('',(1.,0.,0.));
#2625=DIRECTION('',(0.,1.,0.));
#2626=DIRECTION('',(0.,1.,0.));
#2627=DIRECTION('',(1.,0.,0.));
#2628=DIRECTION('',(0.,-1.,0.));
#2629=DIRECTION('',(-1.,0.,0.));
#2630=DIRECTION('',(0.,1.,0.));
#2631=DIRECTION('center_axis',(1.,0.,0.));
#2632=DIRECTION('ref_axis',(0.,1.,0.));
#2633=DIRECTION('',(0.,0.,1.));
#2634=DIRECTION('',(0.,-1.,0.));
#2635=DIRECTION('center_axis',(1.,0.,0.));
#2636=DIRECTION('ref_axis',(0.,1.,0.));
#2637=DIRECTION('',(0.,-1.,0.));
#2638=DIRECTION('',(0.,0.,1.));
#2639=DIRECTION('center_axis',(1.,0.,0.));
#2640=DIRECTION('ref_axis',(0.,1.,0.));
#2641=DIRECTION('',(0.,1.,0.));
#2642=DIRECTION('',(0.,0.,1.));
#2643=DIRECTION('',(0.,1.,0.));
#2644=DIRECTION('',(0.,0.,1.));
#2645=DIRECTION('',(0.,1.,0.));
#2646=DIRECTION('center_axis',(0.,0.,1.));
#2647=DIRECTION('ref_axis',(1.,0.,0.));
#2648=DIRECTION('',(-1.,0.,0.));
#2649=DIRECTION('',(0.,-1.,0.));
#2650=DIRECTION('',(1.,0.,0.));
#2651=DIRECTION('',(-1.,0.,0.));
#2652=DIRECTION('',(0.,1.,0.));
#2653=DIRECTION('',(1.,0.,0.));
#2654=DIRECTION('center_axis',(0.,-1.,0.));
#2655=DIRECTION('ref_axis',(1.,0.,0.));
#2656=DIRECTION('',(0.,0.,1.));
#2657=DIRECTION('center_axis',(0.,1.,0.));
#2658=DIRECTION('ref_axis',(-1.,0.,0.));
#2659=DIRECTION('',(0.,0.,1.));
#2660=DIRECTION('center_axis',(-1.,0.,0.));
#2661=DIRECTION('ref_axis',(0.,-1.,0.));
#2662=DIRECTION('center_axis',(0.,-1.,0.));
#2663=DIRECTION('ref_axis',(1.,0.,0.));
#2664=DIRECTION('',(1.,0.,0.));
#2665=DIRECTION('',(0.,0.,1.));
#2666=DIRECTION('',(0.,0.,1.));
#2667=DIRECTION('center_axis',(1.,0.,0.));
#2668=DIRECTION('ref_axis',(0.,1.,0.));
#2669=DIRECTION('',(0.,1.,0.));
#2670=DIRECTION('',(0.,0.,1.));
#2671=DIRECTION('center_axis',(0.,1.,0.));
#2672=DIRECTION('ref_axis',(-1.,0.,0.));
#2673=DIRECTION('',(-1.,0.,0.));
#2674=DIRECTION('',(0.,0.,1.));
#2675=DIRECTION('center_axis',(-1.,0.,0.));
#2676=DIRECTION('ref_axis',(0.,-1.,0.));
#2677=DIRECTION('',(0.,-1.,0.));
#2678=DIRECTION('center_axis',(0.,1.,0.));
#2679=DIRECTION('ref_axis',(-1.,0.,0.));
#2680=DIRECTION('',(-1.,0.,0.));
#2681=DIRECTION('',(0.,0.,1.));
#2682=DIRECTION('center_axis',(0.,-1.,0.));
#2683=DIRECTION('ref_axis',(1.,0.,0.));
#2684=DIRECTION('',(1.,0.,0.));
#2685=DIRECTION('',(0.,0.,1.));
#2686=DIRECTION('center_axis',(-1.,0.,0.));
#2687=DIRECTION('ref_axis',(0.,-1.,0.));
#2688=DIRECTION('',(0.,-1.,0.));
#2689=DIRECTION('center_axis',(0.,0.,1.));
#2690=DIRECTION('ref_axis',(1.,0.,0.));
#2691=DIRECTION('axis',(0.,0.,1.));
#2692=DIRECTION('refdir',(1.,0.,0.));
#2693=DIRECTION('axis',(0.,0.,1.));
#2694=DIRECTION('refdir',(1.,0.,0.));
#2695=DIRECTION('center_axis',(0.,0.,-1.));
#2696=DIRECTION('ref_axis',(-1.,0.,0.));
#2697=DIRECTION('center_axis',(0.,0.,1.));
#2698=DIRECTION('ref_axis',(1.,0.,0.));
#2699=DIRECTION('center_axis',(0.,0.,1.));
#2700=DIRECTION('ref_axis',(1.,0.,0.));
#2701=DIRECTION('center_axis',(0.,0.,1.));
#2702=DIRECTION('ref_axis',(1.,0.,0.));
#2703=DIRECTION('',(0.707106781186548,8.65956056235494E-17,-0.707106781186547));
#2704=DIRECTION('center_axis',(0.,0.,1.));
#2705=DIRECTION('ref_axis',(1.,0.,0.));
#2706=DIRECTION('center_axis',(0.,0.,1.));
#2707=DIRECTION('ref_axis',(1.,0.,0.));
#2708=DIRECTION('',(0.,0.,-1.));
#2709=DIRECTION('center_axis',(0.,0.,1.));
#2710=DIRECTION('ref_axis',(1.,0.,0.));
#2711=DIRECTION('axis',(0.,0.,1.));
#2712=DIRECTION('refdir',(1.,0.,0.));
#2713=DIRECTION('center_axis',(6.12323399573676E-17,0.,1.));
#2714=DIRECTION('ref_axis',(1.,0.,0.));
#2715=DIRECTION('center_axis',(0.,0.,-1.));
#2716=DIRECTION('ref_axis',(0.,1.,0.));
#2717=DIRECTION('center_axis',(-1.22464679914735E-16,1.,0.));
#2718=DIRECTION('ref_axis',(-1.,-1.22464679914735E-16,0.));
#2719=DIRECTION('center_axis',(0.,0.,-1.));
#2720=DIRECTION('ref_axis',(-1.,0.,0.));
#2721=DIRECTION('center_axis',(0.,0.,1.));
#2722=DIRECTION('ref_axis',(1.,0.,0.));
#2723=DIRECTION('center_axis',(0.,0.,1.));
#2724=DIRECTION('ref_axis',(1.,0.,0.));
#2725=DIRECTION('center_axis',(0.,0.,1.));
#2726=DIRECTION('ref_axis',(1.,0.,0.));
#2727=DIRECTION('',(0.,0.,-1.));
#2728=DIRECTION('center_axis',(0.,0.,-1.));
#2729=DIRECTION('ref_axis',(1.,0.,0.));
#2730=DIRECTION('center_axis',(0.,0.,1.));
#2731=DIRECTION('ref_axis',(1.,0.,0.));
#2732=DIRECTION('',(-0.957826285221151,-1.17299889433528E-16,-0.287347885566345));
#2733=DIRECTION('center_axis',(0.,0.,1.));
#2734=DIRECTION('ref_axis',(1.,0.,0.));
#2735=DIRECTION('axis',(0.,0.,1.));
#2736=DIRECTION('refdir',(1.,0.,0.));
#2737=DIRECTION('center_axis',(0.,0.,1.));
#2738=DIRECTION('ref_axis',(1.,0.,0.));
#2739=DIRECTION('',(0.5,0.866025403784439,0.));
#2740=DIRECTION('',(-0.5,0.866025403784439,0.));
#2741=DIRECTION('',(-1.,1.4792020664489E-16,0.));
#2742=DIRECTION('',(-0.5,-0.866025403784439,0.));
#2743=DIRECTION('',(0.5,-0.866025403784439,0.));
#2744=DIRECTION('',(1.,-2.95840413289779E-16,0.));
#2745=DIRECTION('center_axis',(0.,0.,-1.));
#2746=DIRECTION('ref_axis',(1.,0.,0.));
#2747=DIRECTION('center_axis',(-2.95840413289779E-16,-1.,0.));
#2748=DIRECTION('ref_axis',(1.,-2.95840413289779E-16,0.));
#2749=DIRECTION('',(1.,-2.95840413289779E-16,0.));
#2750=DIRECTION('',(0.,0.,1.));
#2751=DIRECTION('',(0.,0.,1.));
#2752=DIRECTION('center_axis',(-0.866025403784439,-0.5,0.));
#2753=DIRECTION('ref_axis',(0.5,-0.866025403784439,0.));
#2754=DIRECTION('',(0.5,-0.866025403784439,0.));
#2755=DIRECTION('',(0.,0.,1.));
#2756=DIRECTION('center_axis',(-0.866025403784439,0.5,0.));
#2757=DIRECTION('ref_axis',(-0.5,-0.866025403784439,0.));
#2758=DIRECTION('',(-0.5,-0.866025403784439,0.));
#2759=DIRECTION('',(0.,0.,1.));
#2760=DIRECTION('center_axis',(1.4792020664489E-16,1.,0.));
#2761=DIRECTION('ref_axis',(-1.,1.4792020664489E-16,0.));
#2762=DIRECTION('',(-1.,1.4792020664489E-16,0.));
#2763=DIRECTION('',(0.,0.,1.));
#2764=DIRECTION('center_axis',(0.866025403784439,0.5,0.));
#2765=DIRECTION('ref_axis',(-0.5,0.866025403784439,0.));
#2766=DIRECTION('',(-0.5,0.866025403784439,0.));
#2767=DIRECTION('',(0.,0.,1.));
#2768=DIRECTION('center_axis',(0.866025403784439,-0.5,0.));
#2769=DIRECTION('ref_axis',(0.5,0.866025403784439,0.));
#2770=DIRECTION('',(0.5,0.866025403784439,0.));
#2771=DIRECTION('center_axis',(0.,0.,1.));
#2772=DIRECTION('ref_axis',(1.,0.,0.));
#2773=DIRECTION('center_axis',(0.,0.,1.));
#2774=DIRECTION('ref_axis',(1.,0.,0.));
#2775=DIRECTION('',(0.,0.,-1.));
#2776=DIRECTION('center_axis',(0.,0.,-1.));
#2777=DIRECTION('ref_axis',(1.,0.,0.));
#2778=DIRECTION('center_axis',(0.,0.,-1.));
#2779=DIRECTION('ref_axis',(-1.,0.,0.));
#2780=DIRECTION('center_axis',(0.,0.,1.));
#2781=DIRECTION('ref_axis',(1.,0.,0.));
#2782=DIRECTION('center_axis',(0.,0.,-1.));
#2783=DIRECTION('ref_axis',(1.,0.,0.));
#2784=DIRECTION('',(0.,0.,-1.));
#2785=DIRECTION('center_axis',(0.,0.,-1.));
#2786=DIRECTION('ref_axis',(1.,0.,0.));
#2787=DIRECTION('center_axis',(0.,0.,1.));
#2788=DIRECTION('ref_axis',(1.,0.,0.));
#2789=DIRECTION('',(-0.707106781186549,-8.65956056235495E-17,-0.707106781186546));
#2790=DIRECTION('center_axis',(0.,0.,1.));
#2791=DIRECTION('ref_axis',(1.,0.,0.));
#2792=DIRECTION('center_axis',(6.12323399573677E-17,0.,1.));
#2793=DIRECTION('ref_axis',(1.,0.,0.));
#2794=DIRECTION('center_axis',(1.22464679914735E-16,-1.,0.));
#2795=DIRECTION('ref_axis',(-1.,-1.22464679914735E-16,0.));
#2796=DIRECTION('',(0.,0.,1.));
#2797=DIRECTION('',(1.,0.,0.));
#2798=DIRECTION('',(0.,0.,1.));
#2799=DIRECTION('',(1.,0.,0.));
#2800=DIRECTION('',(0.,0.,1.));
#2801=DIRECTION('',(1.,0.,0.));
#2802=DIRECTION('axis',(0.,0.,1.));
#2803=DIRECTION('refdir',(1.,0.,0.));
#2804=DIRECTION('center_axis',(0.,-1.,0.));
#2805=DIRECTION('ref_axis',(1.,0.,0.));
#2806=DIRECTION('center_axis',(0.,1.,0.));
#2807=DIRECTION('ref_axis',(1.,0.,0.));
#2808=DIRECTION('',(0.,1.,0.));
#2809=DIRECTION('center_axis',(0.,-1.,0.));
#2810=DIRECTION('ref_axis',(1.,0.,0.));
#2811=DIRECTION('center_axis',(0.,1.,0.));
#2812=DIRECTION('ref_axis',(1.,0.,0.));
#2813=DIRECTION('center_axis',(0.,-1.,0.));
#2814=DIRECTION('ref_axis',(1.,0.,0.));
#2815=DIRECTION('',(-0.707106781186547,0.707106781186548,-8.65956056235493E-17));
#2816=DIRECTION('center_axis',(0.,-1.,0.));
#2817=DIRECTION('ref_axis',(0.,0.,-1.));
#2818=DIRECTION('center_axis',(0.,-1.,0.));
#2819=DIRECTION('ref_axis',(1.,0.,0.));
#2820=DIRECTION('center_axis',(0.,1.,0.));
#2821=DIRECTION('ref_axis',(1.,0.,0.));
#2822=DIRECTION('',(-0.866025403784439,-0.5,-1.06057523872491E-16));
#2823=DIRECTION('center_axis',(1.92296268638356E-16,0.,-1.));
#2824=DIRECTION('ref_axis',(-1.,0.,-1.92296268638356E-16));
#2825=DIRECTION('',(0.,1.,0.));
#2826=DIRECTION('',(-1.,0.,-1.92296268638356E-16));
#2827=DIRECTION('',(0.,1.,0.));
#2828=DIRECTION('center_axis',(0.866025403784439,0.,-0.5));
#2829=DIRECTION('ref_axis',(-0.5,0.,-0.866025403784439));
#2830=DIRECTION('',(0.,1.,0.));
#2831=DIRECTION('',(-0.5,0.,-0.866025403784439));
#2832=DIRECTION('center_axis',(0.866025403784439,0.,0.5));
#2833=DIRECTION('ref_axis',(0.5,0.,-0.866025403784439));
#2834=DIRECTION('',(0.,1.,0.));
#2835=DIRECTION('',(0.5,0.,-0.866025403784439));
#2836=DIRECTION('center_axis',(-1.92296268638356E-16,0.,1.));
#2837=DIRECTION('ref_axis',(1.,0.,1.92296268638356E-16));
#2838=DIRECTION('',(0.,1.,0.));
#2839=DIRECTION('',(1.,0.,1.92296268638356E-16));
#2840=DIRECTION('center_axis',(-0.866025403784439,0.,0.5));
#2841=DIRECTION('ref_axis',(0.5,0.,0.866025403784439));
#2842=DIRECTION('',(0.,1.,0.));
#2843=DIRECTION('',(0.5,0.,0.866025403784439));
#2844=DIRECTION('center_axis',(-0.866025403784439,0.,-0.5));
#2845=DIRECTION('ref_axis',(-0.5,0.,0.866025403784439));
#2846=DIRECTION('',(-0.5,0.,0.866025403784438));
#2847=DIRECTION('center_axis',(0.,1.,0.));
#2848=DIRECTION('ref_axis',(0.,0.,1.));
#2849=DIRECTION('center_axis',(0.,1.,0.));
#2850=DIRECTION('ref_axis',(1.,0.,0.));
#2851=DIRECTION('',(0.,0.,1.));
#2852=DIRECTION('',(1.,0.,0.));
#2853=DIRECTION('',(0.,0.,1.));
#2854=DIRECTION('',(1.,0.,0.));
#2855=DIRECTION('',(0.,0.,1.));
#2856=DIRECTION('',(1.,0.,0.));
#2857=DIRECTION('',(0.,0.,1.));
#2858=DIRECTION('',(1.,0.,0.));
#2859=DIRECTION('',(0.,0.,1.));
#2860=DIRECTION('',(-1.,1.22464679914735E-16,0.));
#2861=DIRECTION('axis',(0.,0.,1.));
#2862=DIRECTION('refdir',(1.,0.,0.));
#2863=DIRECTION('axis',(0.,0.,1.));
#2864=DIRECTION('refdir',(1.,0.,0.));
#2865=DIRECTION('center_axis',(0.,0.,-1.));
#2866=DIRECTION('ref_axis',(0.,1.,0.));
#2867=DIRECTION('',(0.,1.,0.));
#2868=DIRECTION('',(1.,0.,0.));
#2869=DIRECTION('',(0.,-1.,0.));
#2870=DIRECTION('',(1.,0.,0.));
#2871=DIRECTION('center_axis',(0.,1.,-8.88178419700125E-16));
#2872=DIRECTION('ref_axis',(0.,8.88178419700125E-16,1.));
#2873=DIRECTION('',(0.,8.88178419700125E-16,1.));
#2874=DIRECTION('',(1.,0.,0.));
#2875=DIRECTION('',(0.,-8.88178419700125E-16,-1.));
#2876=DIRECTION('center_axis',(0.,-7.40148683083439E-16,-1.));
#2877=DIRECTION('ref_axis',(0.,1.,-7.40148683083439E-16));
#2878=DIRECTION('',(0.,1.,-7.40148683083439E-16));
#2879=DIRECTION('',(1.,0.,0.));
#2880=DIRECTION('',(0.,-1.,7.40148683083439E-16));
#2881=DIRECTION('center_axis',(0.,-0.707106781186547,-0.707106781186548));
#2882=DIRECTION('ref_axis',(0.,0.707106781186548,-0.707106781186547));
#2883=DIRECTION('',(0.,0.707106781186548,-0.707106781186547));
#2884=DIRECTION('',(1.,0.,0.));
#2885=DIRECTION('',(0.,-0.707106781186548,0.707106781186547));
#2886=DIRECTION('center_axis',(0.,-1.,2.77555756156289E-16));
#2887=DIRECTION('ref_axis',(0.,-2.77555756156289E-16,-1.));
#2888=DIRECTION('',(0.,-2.77555756156289E-16,-1.));
#2889=DIRECTION('',(1.,0.,0.));
#2890=DIRECTION('',(0.,2.77555756156289E-16,1.));
#2891=DIRECTION('center_axis',(0.,-0.707106781186547,0.707106781186548));
#2892=DIRECTION('ref_axis',(0.,-0.707106781186548,-0.707106781186547));
#2893=DIRECTION('',(0.,-0.707106781186548,-0.707106781186547));
#2894=DIRECTION('',(1.,0.,0.));
#2895=DIRECTION('',(0.,0.707106781186548,0.707106781186547));
#2896=DIRECTION('center_axis',(0.,7.40148683083438E-16,1.));
#2897=DIRECTION('ref_axis',(0.,-1.,7.40148683083438E-16));
#2898=DIRECTION('',(0.,-1.,7.40148683083438E-16));
#2899=DIRECTION('',(1.,0.,0.));
#2900=DIRECTION('',(0.,1.,-7.40148683083438E-16));
#2901=DIRECTION('center_axis',(0.,1.,-4.44089209850063E-16));
#2902=DIRECTION('ref_axis',(0.,4.44089209850063E-16,1.));
#2903=DIRECTION('',(0.,4.44089209850063E-16,1.));
#2904=DIRECTION('',(1.,0.,0.));
#2905=DIRECTION('',(0.,-4.44089209850063E-16,-1.));
#2906=DIRECTION('center_axis',(0.,2.41352831440251E-16,1.));
#2907=DIRECTION('ref_axis',(0.,-1.,2.41352831440251E-16));
#2908=DIRECTION('',(0.,-1.,2.41352831440251E-16));
#2909=DIRECTION('',(-1.,0.,0.));
#2910=DIRECTION('',(0.,1.,-2.41352831440251E-16));
#2911=DIRECTION('center_axis',(0.,-1.,2.41352831440251E-16));
#2912=DIRECTION('ref_axis',(0.,-2.41352831440251E-16,-1.));
#2913=DIRECTION('',(0.,-2.41352831440251E-16,-1.));
#2914=DIRECTION('',(1.,0.,0.));
#2915=DIRECTION('',(0.,2.41352831440251E-16,1.));
#2916=DIRECTION('',(1.,0.,0.));
#2917=DIRECTION('center_axis',(0.,0.,-1.));
#2918=DIRECTION('ref_axis',(0.,1.,0.));
#2919=DIRECTION('',(0.,1.,0.));
#2920=DIRECTION('',(1.,0.,0.));
#2921=DIRECTION('',(0.,-1.,0.));
#2922=DIRECTION('center_axis',(0.,-1.,0.));
#2923=DIRECTION('ref_axis',(0.,0.,-1.));
#2924=DIRECTION('',(0.,0.,-1.));
#2925=DIRECTION('',(1.,0.,0.));
#2926=DIRECTION('',(0.,0.,1.));
#2927=DIRECTION('center_axis',(0.,-0.707106781186547,0.707106781186548));
#2928=DIRECTION('ref_axis',(0.,-0.707106781186548,-0.707106781186547));
#2929=DIRECTION('',(0.,-0.707106781186548,-0.707106781186547));
#2930=DIRECTION('',(1.,0.,0.));
#2931=DIRECTION('',(0.,0.707106781186548,0.707106781186547));
#2932=DIRECTION('center_axis',(0.,0.,1.));
#2933=DIRECTION('ref_axis',(0.,-1.,0.));
#2934=DIRECTION('',(0.,-1.,0.));
#2935=DIRECTION('',(1.,0.,0.));
#2936=DIRECTION('',(0.,1.,0.));
#2937=DIRECTION('center_axis',(0.,0.707106781186548,0.707106781186547));
#2938=DIRECTION('ref_axis',(0.,-0.707106781186547,0.707106781186548));
#2939=DIRECTION('',(0.,-0.707106781186547,0.707106781186548));
#2940=DIRECTION('',(1.,0.,0.));
#2941=DIRECTION('',(0.,0.707106781186547,-0.707106781186548));
#2942=DIRECTION('center_axis',(0.,1.,0.));
#2943=DIRECTION('ref_axis',(0.,0.,1.));
#2944=DIRECTION('',(0.,0.,1.));
#2945=DIRECTION('',(1.,0.,0.));
#2946=DIRECTION('',(0.,0.,-1.));
#2947=DIRECTION('center_axis',(0.,0.,-1.));
#2948=DIRECTION('ref_axis',(0.,1.,0.));
#2949=DIRECTION('',(0.,1.,0.));
#2950=DIRECTION('',(1.,0.,0.));
#2951=DIRECTION('',(0.,-1.,0.));
#2952=DIRECTION('center_axis',(0.,1.,-2.41352831440251E-16));
#2953=DIRECTION('ref_axis',(0.,2.41352831440251E-16,1.));
#2954=DIRECTION('',(0.,2.41352831440251E-16,1.));
#2955=DIRECTION('',(-1.,0.,0.));
#2956=DIRECTION('',(0.,-2.41352831440251E-16,-1.));
#2957=DIRECTION('center_axis',(0.,0.,1.));
#2958=DIRECTION('ref_axis',(0.,-1.,0.));
#2959=DIRECTION('',(0.,-1.,0.));
#2960=DIRECTION('',(1.,0.,0.));
#2961=DIRECTION('',(0.,1.,0.));
#2962=DIRECTION('',(1.,0.,0.));
#2963=DIRECTION('center_axis',(0.,-1.,0.));
#2964=DIRECTION('ref_axis',(0.,0.,-1.));
#2965=DIRECTION('',(0.,0.,-1.));
#2966=DIRECTION('',(1.,0.,0.));
#2967=DIRECTION('',(0.,0.,1.));
#2968=DIRECTION('center_axis',(0.,0.,1.));
#2969=DIRECTION('ref_axis',(0.,-1.,0.));
#2970=DIRECTION('',(0.,-1.,0.));
#2971=DIRECTION('',(1.,0.,0.));
#2972=DIRECTION('',(0.,1.,0.));
#2973=DIRECTION('center_axis',(0.,0.707106781186548,0.707106781186548));
#2974=DIRECTION('ref_axis',(0.,-0.707106781186548,0.707106781186548));
#2975=DIRECTION('',(0.,-0.707106781186548,0.707106781186548));
#2976=DIRECTION('',(1.,0.,0.));
#2977=DIRECTION('',(0.,0.707106781186548,-0.707106781186548));
#2978=DIRECTION('center_axis',(0.,1.,0.));
#2979=DIRECTION('ref_axis',(0.,0.,1.));
#2980=DIRECTION('',(0.,0.,1.));
#2981=DIRECTION('',(1.,0.,0.));
#2982=DIRECTION('',(0.,0.,-1.));
#2983=DIRECTION('center_axis',(0.,0.707106781186548,-0.707106781186547));
#2984=DIRECTION('ref_axis',(0.,0.707106781186547,0.707106781186548));
#2985=DIRECTION('',(0.,0.707106781186547,0.707106781186548));
#2986=DIRECTION('',(1.,0.,0.));
#2987=DIRECTION('',(0.,-0.707106781186547,-0.707106781186548));
#2988=DIRECTION('center_axis',(0.,-7.40148683083438E-16,-1.));
#2989=DIRECTION('ref_axis',(0.,1.,-7.40148683083438E-16));
#2990=DIRECTION('',(0.,1.,-7.40148683083438E-16));
#2991=DIRECTION('',(1.,0.,0.));
#2992=DIRECTION('',(0.,-1.,7.40148683083438E-16));
#2993=DIRECTION('center_axis',(0.,-1.,0.));
#2994=DIRECTION('ref_axis',(0.,0.,-1.));
#2995=DIRECTION('',(0.,0.,-1.));
#2996=DIRECTION('',(1.,0.,0.));
#2997=DIRECTION('',(0.,0.,1.));
#2998=DIRECTION('center_axis',(0.,0.,-1.));
#2999=DIRECTION('ref_axis',(0.,1.,0.));
#3000=DIRECTION('',(0.,1.,0.));
#3001=DIRECTION('',(-1.,0.,0.));
#3002=DIRECTION('',(0.,-1.,0.));
#3003=DIRECTION('center_axis',(0.,1.,0.));
#3004=DIRECTION('ref_axis',(0.,0.,1.));
#3005=DIRECTION('',(0.,0.,1.));
#3006=DIRECTION('',(1.,0.,0.));
#3007=DIRECTION('',(0.,0.,-1.));
#3008=DIRECTION('',(1.,0.,0.));
#3009=DIRECTION('center_axis',(0.,0.,1.));
#3010=DIRECTION('ref_axis',(0.,-1.,0.));
#3011=DIRECTION('',(0.,-1.,0.));
#3012=DIRECTION('',(1.,0.,0.));
#3013=DIRECTION('',(0.,1.,0.));
#3014=DIRECTION('center_axis',(0.,1.,0.));
#3015=DIRECTION('ref_axis',(0.,0.,1.));
#3016=DIRECTION('',(0.,0.,1.));
#3017=DIRECTION('',(1.,0.,0.));
#3018=DIRECTION('',(0.,0.,-1.));
#3019=DIRECTION('center_axis',(0.,0.707106781186547,-0.707106781186548));
#3020=DIRECTION('ref_axis',(0.,0.707106781186548,0.707106781186547));
#3021=DIRECTION('',(0.,0.707106781186548,0.707106781186547));
#3022=DIRECTION('',(1.,0.,0.));
#3023=DIRECTION('',(0.,-0.707106781186548,-0.707106781186547));
#3024=DIRECTION('center_axis',(0.,0.,-1.));
#3025=DIRECTION('ref_axis',(0.,1.,0.));
#3026=DIRECTION('',(0.,1.,0.));
#3027=DIRECTION('',(1.,0.,0.));
#3028=DIRECTION('',(0.,-1.,0.));
#3029=DIRECTION('center_axis',(0.,-0.707106781186547,-0.707106781186548));
#3030=DIRECTION('ref_axis',(0.,0.707106781186548,-0.707106781186547));
#3031=DIRECTION('',(0.,0.707106781186548,-0.707106781186547));
#3032=DIRECTION('',(1.,0.,0.));
#3033=DIRECTION('',(0.,-0.707106781186548,0.707106781186547));
#3034=DIRECTION('center_axis',(0.,-1.,0.));
#3035=DIRECTION('ref_axis',(0.,0.,-1.));
#3036=DIRECTION('',(0.,0.,-1.));
#3037=DIRECTION('',(1.,0.,0.));
#3038=DIRECTION('',(0.,0.,1.));
#3039=DIRECTION('center_axis',(0.,0.,1.));
#3040=DIRECTION('ref_axis',(0.,-1.,0.));
#3041=DIRECTION('',(0.,-1.,0.));
#3042=DIRECTION('',(1.,0.,0.));
#3043=DIRECTION('',(0.,1.,0.));
#3044=DIRECTION('center_axis',(0.,-1.,0.));
#3045=DIRECTION('ref_axis',(0.,0.,-1.));
#3046=DIRECTION('',(0.,0.,-1.));
#3047=DIRECTION('',(-1.,0.,0.));
#3048=DIRECTION('',(0.,0.,1.));
#3049=DIRECTION('center_axis',(1.,0.,0.));
#3050=DIRECTION('ref_axis',(0.,0.,-1.));
#3051=DIRECTION('center_axis',(1.,0.,0.));
#3052=DIRECTION('ref_axis',(0.,0.,-1.));
#3053=DIRECTION('',(1.,0.,0.));
#3054=DIRECTION('center_axis',(-1.,0.,0.));
#3055=DIRECTION('ref_axis',(0.,0.,-1.));
#3056=DIRECTION('center_axis',(0.,1.,0.));
#3057=DIRECTION('ref_axis',(0.,0.,1.));
#3058=DIRECTION('',(0.,0.,1.));
#3059=DIRECTION('',(1.,0.,0.));
#3060=DIRECTION('',(0.,0.,1.));
#3061=DIRECTION('center_axis',(0.,1.,0.));
#3062=DIRECTION('ref_axis',(0.,0.,1.));
#3063=DIRECTION('',(0.,0.,1.));
#3064=DIRECTION('',(1.,0.,0.));
#3065=DIRECTION('',(0.,0.,1.));
#3066=DIRECTION('center_axis',(0.,0.,-1.));
#3067=DIRECTION('ref_axis',(0.,1.,0.));
#3068=DIRECTION('',(0.,1.,0.));
#3069=DIRECTION('',(0.,1.,0.));
#3070=DIRECTION('center_axis',(0.,0.,-1.));
#3071=DIRECTION('ref_axis',(0.,1.,0.));
#3072=DIRECTION('',(0.,1.,0.));
#3073=DIRECTION('',(1.,0.,0.));
#3074=DIRECTION('',(0.,1.,0.));
#3075=DIRECTION('center_axis',(0.,-1.,0.));
#3076=DIRECTION('ref_axis',(0.,0.,-1.));
#3077=DIRECTION('',(0.,0.,-1.));
#3078=DIRECTION('',(0.,0.,-1.));
#3079=DIRECTION('center_axis',(0.,-1.,0.));
#3080=DIRECTION('ref_axis',(0.,0.,-1.));
#3081=DIRECTION('',(0.,0.,-1.));
#3082=DIRECTION('',(1.,0.,0.));
#3083=DIRECTION('',(0.,0.,-1.));
#3084=DIRECTION('center_axis',(0.,0.,1.));
#3085=DIRECTION('ref_axis',(0.,-1.,0.));
#3086=DIRECTION('',(0.,-1.,0.));
#3087=DIRECTION('',(0.,-1.,0.));
#3088=DIRECTION('center_axis',(0.,0.,1.));
#3089=DIRECTION('ref_axis',(0.,-1.,0.));
#3090=DIRECTION('',(0.,-1.,0.));
#3091=DIRECTION('',(0.,-1.,0.));
#3092=DIRECTION('center_axis',(1.,0.,0.));
#3093=DIRECTION('ref_axis',(0.,0.,-1.));
#3094=DIRECTION('center_axis',(1.,0.,0.));
#3095=DIRECTION('ref_axis',(0.,0.,-1.));
#3096=DIRECTION('',(-1.,0.,2.22044604925031E-16));
#3097=DIRECTION('',(2.22044604925031E-16,0.,1.));
#3098=DIRECTION('',(0.,0.,1.));
#3099=DIRECTION('',(1.,0.,0.));
#3100=DIRECTION('',(0.,0.,1.));
#3101=DIRECTION('',(1.,0.,0.));
#3102=CARTESIAN_POINT('',(0.,0.,0.));
#3103=CARTESIAN_POINT('',(0.,0.,0.));
#3104=CARTESIAN_POINT('',(0.,0.,0.));
#3105=CARTESIAN_POINT('Origin',(0.,0.,5.9));
#3106=CARTESIAN_POINT('',(-0.34,-4.163799117101E-17,6.));
#3107=CARTESIAN_POINT('Origin',(0.,0.,6.));
#3108=CARTESIAN_POINT('',(-0.34,4.163799117101E-17,7.));
#3109=CARTESIAN_POINT('',(-0.34,-4.163799117101E-17,5.9));
#3110=CARTESIAN_POINT('Origin',(0.,0.,7.));
#3111=CARTESIAN_POINT('Origin',(2.2,2.2,6.));
#3112=CARTESIAN_POINT('',(2.2,2.2,6.));
#3113=CARTESIAN_POINT('',(-2.2,2.2,6.));
#3114=CARTESIAN_POINT('',(2.2,2.2,6.));
#3115=CARTESIAN_POINT('',(-2.2,2.2,7.));
#3116=CARTESIAN_POINT('',(-2.2,2.2,6.));
#3117=CARTESIAN_POINT('',(2.2,2.2,7.));
#3118=CARTESIAN_POINT('',(2.2,2.2,7.));
#3119=CARTESIAN_POINT('',(2.2,2.2,6.));
#3120=CARTESIAN_POINT('Origin',(2.2,-2.2,6.));
#3121=CARTESIAN_POINT('',(2.2,-2.2,6.));
#3122=CARTESIAN_POINT('',(2.2,-2.2,6.));
#3123=CARTESIAN_POINT('',(2.2,-2.2,7.));
#3124=CARTESIAN_POINT('',(2.2,-2.2,7.));
#3125=CARTESIAN_POINT('',(2.2,-2.2,6.));
#3126=CARTESIAN_POINT('Origin',(-2.2,-2.2,6.));
#3127=CARTESIAN_POINT('',(-2.2,-2.2,6.));
#3128=CARTESIAN_POINT('',(-2.2,-2.2,6.));
#3129=CARTESIAN_POINT('',(-2.2,-2.2,7.));
#3130=CARTESIAN_POINT('',(-2.2,-2.2,7.));
#3131=CARTESIAN_POINT('',(-2.2,-2.2,6.));
#3132=CARTESIAN_POINT('Origin',(-2.2,2.2,6.));
#3133=CARTESIAN_POINT('',(-2.2,2.2,6.));
#3134=CARTESIAN_POINT('',(-2.2,2.2,7.));
#3135=CARTESIAN_POINT('Origin',(0.,0.,7.));
#3136=CARTESIAN_POINT('Origin',(0.,0.,6.));
#3137=CARTESIAN_POINT('',(0.,0.,0.));
#3138=CARTESIAN_POINT('Origin',(-1.01,-1.01,6.9));
#3139=CARTESIAN_POINT('',(1.01,-1.01,27.));
#3140=CARTESIAN_POINT('',(-1.01,-1.01,27.));
#3141=CARTESIAN_POINT('',(-0.505,-1.01,27.));
#3142=CARTESIAN_POINT('',(1.01,-1.01,7.));
#3143=CARTESIAN_POINT('',(1.01,-1.01,6.9));
#3144=CARTESIAN_POINT('',(-1.01,-1.01,7.));
#3145=CARTESIAN_POINT('',(-0.505,-1.01,7.));
#3146=CARTESIAN_POINT('',(-1.01,-1.01,6.9));
#3147=CARTESIAN_POINT('Origin',(-1.01,1.01,6.9));
#3148=CARTESIAN_POINT('',(-1.01,1.01,27.));
#3149=CARTESIAN_POINT('',(-1.01,0.505,27.));
#3150=CARTESIAN_POINT('',(-1.01,1.01,7.));
#3151=CARTESIAN_POINT('',(-1.01,0.505,7.));
#3152=CARTESIAN_POINT('',(-1.01,1.01,6.9));
#3153=CARTESIAN_POINT('Origin',(1.01,1.01,6.9));
#3154=CARTESIAN_POINT('',(1.01,1.01,27.));
#3155=CARTESIAN_POINT('',(0.505,1.01,27.));
#3156=CARTESIAN_POINT('',(1.01,1.01,7.));
#3157=CARTESIAN_POINT('',(0.505,1.01,7.));
#3158=CARTESIAN_POINT('',(1.01,1.01,6.9));
#3159=CARTESIAN_POINT('Origin',(1.01,-1.01,6.9));
#3160=CARTESIAN_POINT('',(1.01,-0.505,27.));
#3161=CARTESIAN_POINT('',(1.01,-0.505,7.));
#3162=CARTESIAN_POINT('Origin',(1.5,1.5,7.));
#3163=CARTESIAN_POINT('',(1.5,1.5,7.));
#3164=CARTESIAN_POINT('',(-1.5,1.5,7.));
#3165=CARTESIAN_POINT('',(1.5,1.5,7.));
#3166=CARTESIAN_POINT('',(-1.5,1.5,27.));
#3167=CARTESIAN_POINT('',(-1.5,1.5,7.));
#3168=CARTESIAN_POINT('',(1.5,1.5,27.));
#3169=CARTESIAN_POINT('',(1.5,1.5,27.));
#3170=CARTESIAN_POINT('',(1.5,1.5,7.));
#3171=CARTESIAN_POINT('Origin',(1.5,-1.5,7.));
#3172=CARTESIAN_POINT('',(1.5,-1.5,7.));
#3173=CARTESIAN_POINT('',(1.5,-1.5,7.));
#3174=CARTESIAN_POINT('',(1.5,-1.5,27.));
#3175=CARTESIAN_POINT('',(1.5,-1.5,27.));
#3176=CARTESIAN_POINT('',(1.5,-1.5,7.));
#3177=CARTESIAN_POINT('Origin',(-1.5,-1.5,7.));
#3178=CARTESIAN_POINT('',(-1.5,-1.5,7.));
#3179=CARTESIAN_POINT('',(-1.5,-1.5,7.));
#3180=CARTESIAN_POINT('',(-1.5,-1.5,27.));
#3181=CARTESIAN_POINT('',(-1.5,-1.5,27.));
#3182=CARTESIAN_POINT('',(-1.5,-1.5,7.));
#3183=CARTESIAN_POINT('Origin',(-1.5,1.5,7.));
#3184=CARTESIAN_POINT('',(-1.5,1.5,7.));
#3185=CARTESIAN_POINT('',(-1.5,1.5,27.));
#3186=CARTESIAN_POINT('Origin',(0.,0.,27.));
#3187=CARTESIAN_POINT('Origin',(0.,0.,7.));
#3188=CARTESIAN_POINT('',(0.,0.,0.));
#3189=CARTESIAN_POINT('Origin',(1.6,0.05,28.));
#3190=CARTESIAN_POINT('',(1.35,0.05,28.));
#3191=CARTESIAN_POINT('Origin',(1.6,0.05,28.));
#3192=CARTESIAN_POINT('',(1.35,1.8,28.));
#3193=CARTESIAN_POINT('',(1.35,0.05,28.));
#3194=CARTESIAN_POINT('Origin',(1.6,1.8,28.));
#3195=CARTESIAN_POINT('Origin',(1.6,-1.9,28.));
#3196=CARTESIAN_POINT('',(1.27,-1.8,28.));
#3197=CARTESIAN_POINT('Origin',(1.6,-1.8,28.));
#3198=CARTESIAN_POINT('',(1.27,-0.05,28.));
#3199=CARTESIAN_POINT('',(1.27,-1.9,28.));
#3200=CARTESIAN_POINT('Origin',(1.6,-0.05,28.));
#3201=CARTESIAN_POINT('Origin',(2.3,0.05,27.));
#3202=CARTESIAN_POINT('',(1.01,0.05,27.));
#3203=CARTESIAN_POINT('',(1.01,0.05,29.));
#3204=CARTESIAN_POINT('',(1.01,0.05,26.95));
#3205=CARTESIAN_POINT('',(1.51,0.05,27.));
#3206=CARTESIAN_POINT('',(1.15,0.05,27.));
#3207=CARTESIAN_POINT('',(2.2,0.05,27.));
#3208=CARTESIAN_POINT('',(2.3,0.05,27.));
#3209=CARTESIAN_POINT('',(2.2,0.05,29.));
#3210=CARTESIAN_POINT('',(2.2,0.05,26.5));
#3211=CARTESIAN_POINT('',(1.15,0.05,29.));
#3212=CARTESIAN_POINT('Origin',(0.,-0.05,27.));
#3213=CARTESIAN_POINT('',(1.01,-0.05,29.));
#3214=CARTESIAN_POINT('',(1.01,-0.05,27.));
#3215=CARTESIAN_POINT('',(1.01,-0.05,26.95));
#3216=CARTESIAN_POINT('',(2.2,-0.05,29.));
#3217=CARTESIAN_POINT('',(0.,-0.05,29.));
#3218=CARTESIAN_POINT('',(2.2,-0.05,27.));
#3219=CARTESIAN_POINT('',(2.2,-0.05,26.5));
#3220=CARTESIAN_POINT('',(1.51,-0.05,27.));
#3221=CARTESIAN_POINT('',(0.,-0.05,27.));
#3222=CARTESIAN_POINT('',(0.,-0.05,27.));
#3223=CARTESIAN_POINT('Origin',(1.15,0.,27.));
#3224=CARTESIAN_POINT('',(1.51,-1.51,27.));
#3225=CARTESIAN_POINT('',(2.2,-0.9,27.));
#3226=CARTESIAN_POINT('Origin',(0.,0.,27.));
#3227=CARTESIAN_POINT('',(1.01,1.01,27.));
#3228=CARTESIAN_POINT('',(1.01,-0.505,27.));
#3229=CARTESIAN_POINT('',(-1.01,1.01,27.));
#3230=CARTESIAN_POINT('',(0.505,1.01,27.));
#3231=CARTESIAN_POINT('',(-1.01,-1.01,27.));
#3232=CARTESIAN_POINT('',(-1.01,0.505,27.));
#3233=CARTESIAN_POINT('',(1.01,-1.01,27.));
#3234=CARTESIAN_POINT('',(-0.505,-1.01,27.));
#3235=CARTESIAN_POINT('',(1.01,-0.505,27.));
#3236=CARTESIAN_POINT('',(1.51,-1.51,27.));
#3237=CARTESIAN_POINT('',(1.51,-1.51,27.));
#3238=CARTESIAN_POINT('',(-1.51,-1.51,27.));
#3239=CARTESIAN_POINT('',(-1.51,-1.51,27.));
#3240=CARTESIAN_POINT('',(-1.51,1.51,27.));
#3241=CARTESIAN_POINT('',(-1.51,1.51,27.));
#3242=CARTESIAN_POINT('',(1.51,1.51,27.));
#3243=CARTESIAN_POINT('',(1.51,1.51,27.));
#3244=CARTESIAN_POINT('',(1.51,-1.51,27.));
#3245=CARTESIAN_POINT('Origin',(1.01,-1.01,26.9));
#3246=CARTESIAN_POINT('',(1.01,-1.01,29.));
#3247=CARTESIAN_POINT('',(1.01,-1.01,26.9));
#3248=CARTESIAN_POINT('',(1.01,-0.505,29.));
#3249=CARTESIAN_POINT('Origin',(1.01,-1.01,26.9));
#3250=CARTESIAN_POINT('',(1.01,1.01,29.));
#3251=CARTESIAN_POINT('',(1.01,-0.505,29.));
#3252=CARTESIAN_POINT('',(1.01,1.01,26.9));
#3253=CARTESIAN_POINT('Origin',(2.2,-1.8,26.));
#3254=CARTESIAN_POINT('',(2.2,-1.8,29.));
#3255=CARTESIAN_POINT('',(2.2,-1.8,29.));
#3256=CARTESIAN_POINT('',(2.2,-1.8,26.));
#3257=CARTESIAN_POINT('',(2.2,-1.8,26.));
#3258=CARTESIAN_POINT('',(2.2,1.8,26.));
#3259=CARTESIAN_POINT('',(2.2,-1.8,26.));
#3260=CARTESIAN_POINT('',(2.2,1.8,29.));
#3261=CARTESIAN_POINT('',(2.2,1.8,26.));
#3262=CARTESIAN_POINT('',(2.2,-1.8,29.));
#3263=CARTESIAN_POINT('Origin',(0.,0.,29.));
#3264=CARTESIAN_POINT('',(-2.2,1.8,29.));
#3265=CARTESIAN_POINT('',(2.2,1.8,29.));
#3266=CARTESIAN_POINT('',(-2.2,-1.8,29.));
#3267=CARTESIAN_POINT('',(-2.2,1.8,29.));
#3268=CARTESIAN_POINT('',(-2.2,-1.8,29.));
#3269=CARTESIAN_POINT('',(-1.01,-1.01,29.));
#3270=CARTESIAN_POINT('',(-0.505,-1.01,29.));
#3271=CARTESIAN_POINT('',(-1.01,1.01,29.));
#3272=CARTESIAN_POINT('',(-1.01,0.505,29.));
#3273=CARTESIAN_POINT('',(0.505,1.01,29.));
#3274=CARTESIAN_POINT('Origin',(-1.01,-1.01,26.9));
#3275=CARTESIAN_POINT('',(-1.01,-1.01,26.9));
#3276=CARTESIAN_POINT('Origin',(1.01,1.01,26.9));
#3277=CARTESIAN_POINT('',(-1.01,1.01,26.9));
#3278=CARTESIAN_POINT('Origin',(-1.01,1.01,26.9));
#3279=CARTESIAN_POINT('Origin',(-1.51,-1.51,25.9));
#3280=CARTESIAN_POINT('',(-1.51,-1.51,26.));
#3281=CARTESIAN_POINT('',(1.51,-1.51,26.));
#3282=CARTESIAN_POINT('',(-0.755,-1.51,26.));
#3283=CARTESIAN_POINT('',(-1.51,-1.51,25.9));
#3284=CARTESIAN_POINT('',(1.51,-1.51,25.9));
#3285=CARTESIAN_POINT('Origin',(1.51,-1.51,25.9));
#3286=CARTESIAN_POINT('',(1.51,1.51,26.));
#3287=CARTESIAN_POINT('',(1.51,-0.755,26.));
#3288=CARTESIAN_POINT('',(1.51,1.51,25.9));
#3289=CARTESIAN_POINT('Origin',(1.51,1.51,25.9));
#3290=CARTESIAN_POINT('',(-1.51,1.51,26.));
#3291=CARTESIAN_POINT('',(0.755,1.51,26.));
#3292=CARTESIAN_POINT('',(-1.51,1.51,25.9));
#3293=CARTESIAN_POINT('Origin',(-1.51,1.51,25.9));
#3294=CARTESIAN_POINT('',(-1.51,0.755,26.));
#3295=CARTESIAN_POINT('Origin',(2.2,1.8,26.));
#3296=CARTESIAN_POINT('',(-2.2,1.8,26.));
#3297=CARTESIAN_POINT('',(2.2,1.8,26.));
#3298=CARTESIAN_POINT('',(-2.2,1.8,26.));
#3299=CARTESIAN_POINT('Origin',(-2.2,-1.8,26.));
#3300=CARTESIAN_POINT('',(-2.2,-1.8,26.));
#3301=CARTESIAN_POINT('',(-2.2,-1.8,26.));
#3302=CARTESIAN_POINT('',(-2.2,-1.8,26.));
#3303=CARTESIAN_POINT('Origin',(-2.2,1.8,26.));
#3304=CARTESIAN_POINT('',(-2.2,1.8,26.));
#3305=CARTESIAN_POINT('Origin',(0.,0.,26.));
#3306=CARTESIAN_POINT('',(0.,0.,0.));
#3307=CARTESIAN_POINT('',(0.,0.,0.));
#3308=CARTESIAN_POINT('Origin',(1.9,0.,0.));
#3309=CARTESIAN_POINT('',(-1.9,-2.32682891837997E-16,-4.16333634234434E-17));
#3310=CARTESIAN_POINT('Origin',(0.,0.,0.));
#3311=CARTESIAN_POINT('Origin',(0.,0.,0.05));
#3312=CARTESIAN_POINT('',(-2.,-2.44929359829471E-16,0.1));
#3313=CARTESIAN_POINT('Origin',(0.,0.,0.1));
#3314=CARTESIAN_POINT('',(-1.95,-2.38806125833734E-16,0.05));
#3315=CARTESIAN_POINT('Origin',(0.,0.,0.25));
#3316=CARTESIAN_POINT('',(-2.,-2.44929359829471E-16,0.4));
#3317=CARTESIAN_POINT('Origin',(0.,0.,0.4));
#3318=CARTESIAN_POINT('',(-2.,-2.44929359829471E-16,0.25));
#3319=CARTESIAN_POINT('Origin',(0.,0.,0.4));
#3320=CARTESIAN_POINT('',(0.,0.,0.));
#3321=CARTESIAN_POINT('Origin',(1.11022302462516E-16,0.,1.1));
#3322=CARTESIAN_POINT('',(-0.48,-5.8783046359073E-17,1.3));
#3323=CARTESIAN_POINT('Origin',(1.11022302462516E-16,0.,1.3));
#3324=CARTESIAN_POINT('',(7.91814856846845E-17,-3.89937543492083E-33,0.58));
#3325=CARTESIAN_POINT('Origin',(1.11022302462516E-16,0.,1.1));
#3326=CARTESIAN_POINT('Origin',(2.,0.,0.4));
#3327=CARTESIAN_POINT('',(-2.,-2.44929359829471E-16,0.4));
#3328=CARTESIAN_POINT('Origin',(0.,0.,0.4));
#3329=CARTESIAN_POINT('Origin',(0.,0.,0.7));
#3330=CARTESIAN_POINT('',(-2.,-2.44929359829471E-16,1.));
#3331=CARTESIAN_POINT('Origin',(0.,0.,1.));
#3332=CARTESIAN_POINT('',(-2.,-2.44929359829471E-16,0.7));
#3333=CARTESIAN_POINT('Origin',(0.,0.,1.15));
#3334=CARTESIAN_POINT('',(-1.,-1.22464679914735E-16,1.3));
#3335=CARTESIAN_POINT('Origin',(0.,0.,1.3));
#3336=CARTESIAN_POINT('',(-1.5,-1.83697019872103E-16,1.15));
#3337=CARTESIAN_POINT('Origin',(0.,0.,1.3));
#3338=CARTESIAN_POINT('',(0.,0.,0.));
#3339=CARTESIAN_POINT('Origin',(0.,1.11022302462516E-16,2.5));
#3340=CARTESIAN_POINT('',(0.375277674973257,-0.65,2.5));
#3341=CARTESIAN_POINT('',(0.750555349946514,0.,2.5));
#3342=CARTESIAN_POINT('',(0.375277674973257,-0.65,2.5));
#3343=CARTESIAN_POINT('',(0.375277674973257,0.65,2.5));
#3344=CARTESIAN_POINT('',(0.750555349946514,0.,2.5));
#3345=CARTESIAN_POINT('',(-0.375277674973257,0.65,2.5));
#3346=CARTESIAN_POINT('',(0.375277674973257,0.65,2.5));
#3347=CARTESIAN_POINT('',(-0.750555349946514,1.11022302462516E-16,2.5));
#3348=CARTESIAN_POINT('',(-0.375277674973257,0.65,2.5));
#3349=CARTESIAN_POINT('',(-0.375277674973257,-0.65,2.5));
#3350=CARTESIAN_POINT('',(-0.750555349946514,9.19165206894919E-17,2.5));
#3351=CARTESIAN_POINT('',(-0.375277674973257,-0.65,2.5));
#3352=CARTESIAN_POINT('',(-0.3933,4.81653586104654E-17,2.5));
#3353=CARTESIAN_POINT('Origin',(0.,0.,2.5));
#3354=CARTESIAN_POINT('Origin',(-0.375277674973257,-0.65,1.8));
#3355=CARTESIAN_POINT('',(-0.375277674973257,-0.65,1.8));
#3356=CARTESIAN_POINT('',(0.375277674973257,-0.65,1.8));
#3357=CARTESIAN_POINT('',(-0.375277674973257,-0.65,1.8));
#3358=CARTESIAN_POINT('',(0.375277674973257,-0.65,1.8));
#3359=CARTESIAN_POINT('',(-0.375277674973257,-0.65,1.8));
#3360=CARTESIAN_POINT('Origin',(-0.750555349946514,9.19165206894919E-17,
1.8));
#3361=CARTESIAN_POINT('',(-0.750555349946514,9.19165206894919E-17,1.8));
#3362=CARTESIAN_POINT('',(-0.750555349946514,9.19165206894919E-17,1.8));
#3363=CARTESIAN_POINT('',(-0.750555349946514,9.19165206894919E-17,1.8));
#3364=CARTESIAN_POINT('Origin',(-0.375277674973257,0.65,1.8));
#3365=CARTESIAN_POINT('',(-0.375277674973257,0.65,1.8));
#3366=CARTESIAN_POINT('',(-0.375277674973257,0.65,1.8));
#3367=CARTESIAN_POINT('',(-0.375277674973257,0.65,1.8));
#3368=CARTESIAN_POINT('Origin',(0.375277674973257,0.65,1.8));
#3369=CARTESIAN_POINT('',(0.375277674973257,0.65,1.8));
#3370=CARTESIAN_POINT('',(0.375277674973257,0.65,1.8));
#3371=CARTESIAN_POINT('',(0.375277674973257,0.65,1.8));
#3372=CARTESIAN_POINT('Origin',(0.750555349946514,0.,1.8));
#3373=CARTESIAN_POINT('',(0.750555349946514,0.,1.8));
#3374=CARTESIAN_POINT('',(0.750555349946514,0.,1.8));
#3375=CARTESIAN_POINT('',(0.750555349946514,0.,1.8));
#3376=CARTESIAN_POINT('Origin',(0.375277674973257,-0.65,1.8));
#3377=CARTESIAN_POINT('',(0.375277674973257,-0.65,1.8));
#3378=CARTESIAN_POINT('Origin',(0.,0.,1.45));
#3379=CARTESIAN_POINT('',(-0.3,-3.67394039744206E-17,1.8));
#3380=CARTESIAN_POINT('Origin',(0.,0.,1.8));
#3381=CARTESIAN_POINT('',(-0.3,3.67394039744206E-17,1.5));
#3382=CARTESIAN_POINT('',(-0.3,-3.67394039744206E-17,1.45));
#3383=CARTESIAN_POINT('Origin',(0.,0.,1.5));
#3384=CARTESIAN_POINT('Origin',(0.4,0.,1.8));
#3385=CARTESIAN_POINT('Origin',(0.,0.,4.6));
#3386=CARTESIAN_POINT('',(-0.3933,4.81653586104654E-17,7.4067));
#3387=CARTESIAN_POINT('Origin',(0.,0.,7.4067));
#3388=CARTESIAN_POINT('',(-0.3933,-4.81653586104654E-17,4.6));
#3389=CARTESIAN_POINT('Origin',(0.,0.,7.45));
#3390=CARTESIAN_POINT('',(-0.3,-3.67394039744206E-17,7.5));
#3391=CARTESIAN_POINT('Origin',(0.,0.,7.5));
#3392=CARTESIAN_POINT('',(-0.35,-4.28626379701574E-17,7.45));
#3393=CARTESIAN_POINT('Origin',(0.,0.,7.5));
#3394=CARTESIAN_POINT('Origin',(-5.55111512312578E-17,0.,1.1));
#3395=CARTESIAN_POINT('',(-8.61273212099417E-17,-3.74939945665464E-33,0.6));
#3396=CARTESIAN_POINT('Origin',(-5.55111512312578E-17,0.,1.1));
#3397=CARTESIAN_POINT('',(0.,0.,0.));
#3398=CARTESIAN_POINT('',(0.,0.,0.));
#3399=CARTESIAN_POINT('',(0.,0.,0.));
#3400=CARTESIAN_POINT('',(0.,0.,0.));
#3401=CARTESIAN_POINT('Origin',(0.,-1.445,0.));
#3402=CARTESIAN_POINT('',(-0.2942,-2.9458,3.60291088309151E-17));
#3403=CARTESIAN_POINT('Origin',(0.,-2.9458,0.));
#3404=CARTESIAN_POINT('',(-0.2942,0.,-3.60291088309151E-17));
#3405=CARTESIAN_POINT('',(-0.2942,-1.445,-3.60291088309151E-17));
#3406=CARTESIAN_POINT('Origin',(0.,0.,0.));
#3407=CARTESIAN_POINT('Origin',(0.,-2.97,0.));
#3408=CARTESIAN_POINT('',(-0.24,-3.,-2.93915231795365E-17));
#3409=CARTESIAN_POINT('Origin',(0.,-3.,0.));
#3410=CARTESIAN_POINT('',(-0.27,-2.97,-3.30654635769785E-17));
#3411=CARTESIAN_POINT('Origin',(0.,-3.,0.));
#3412=CARTESIAN_POINT('Origin',(0.,0.341586508806388,0.));
#3413=CARTESIAN_POINT('',(-0.475,0.4,-5.81707229594993E-17));
#3414=CARTESIAN_POINT('Origin',(0.,0.4,0.));
#3415=CARTESIAN_POINT('',(-0.577350269189626,0.340908044531739,-7.07050159149938E-17));
#3416=CARTESIAN_POINT('',(-0.576175134594813,0.341586508806388,-7.05611034329833E-17));
#3417=CARTESIAN_POINT('',(-0.288675134594813,0.340908044531739,0.5));
#3418=CARTESIAN_POINT('Ctrl Pts',(-0.288675134594813,0.340908044531739,
0.5));
#3419=CARTESIAN_POINT('Ctrl Pts',(-0.433012701893303,0.424241377863696,
0.249999999998124));
#3420=CARTESIAN_POINT('Ctrl Pts',(-0.577350269189626,0.340908044531739,
-7.07050159149938E-17));
#3421=CARTESIAN_POINT('',(0.288675134594813,0.340908044531739,0.5));
#3422=CARTESIAN_POINT('Ctrl Pts',(0.288675134594813,0.340908044531739,0.5));
#3423=CARTESIAN_POINT('Ctrl Pts',(-2.16648921025353E-12,0.424241377863696,
0.5));
#3424=CARTESIAN_POINT('Ctrl Pts',(-0.288675134594813,0.340908044531739,
0.5));
#3425=CARTESIAN_POINT('',(0.577350269189626,0.340908044531739,0.));
#3426=CARTESIAN_POINT('Ctrl Pts',(0.577350269189626,0.340908044531739,0.));
#3427=CARTESIAN_POINT('Ctrl Pts',(0.433012701891136,0.424241377863697,0.250000000001876));
#3428=CARTESIAN_POINT('Ctrl Pts',(0.288675134594813,0.340908044531739,0.5));
#3429=CARTESIAN_POINT('',(0.288675134594813,0.340908044531739,-0.5));
#3430=CARTESIAN_POINT('Ctrl Pts',(0.288675134594813,0.340908044531739,-0.5));
#3431=CARTESIAN_POINT('Ctrl Pts',(0.433012701893303,0.424241377863696,-0.249999999998124));
#3432=CARTESIAN_POINT('Ctrl Pts',(0.577350269189626,0.340908044531739,0.));
#3433=CARTESIAN_POINT('',(-0.288675134594813,0.340908044531739,-0.5));
#3434=CARTESIAN_POINT('Ctrl Pts',(-0.288675134594813,0.340908044531739,
-0.5));
#3435=CARTESIAN_POINT('Ctrl Pts',(2.16660023255599E-12,0.424241377863696,
-0.5));
#3436=CARTESIAN_POINT('Ctrl Pts',(0.288675134594813,0.340908044531739,-0.5));
#3437=CARTESIAN_POINT('Ctrl Pts',(-0.577350269189626,0.340908044531739,
-7.07050159149938E-17));
#3438=CARTESIAN_POINT('Ctrl Pts',(-0.433012701891136,0.424241377863697,
-0.250000000001876));
#3439=CARTESIAN_POINT('Ctrl Pts',(-0.288675134594813,0.340908044531739,
-0.5));
#3440=CARTESIAN_POINT('Origin',(0.288675134594813,0.,-0.5));
#3441=CARTESIAN_POINT('',(0.288675134594813,0.,-0.5));
#3442=CARTESIAN_POINT('',(0.288675134594813,0.,-0.5));
#3443=CARTESIAN_POINT('',(-0.288675134594813,0.,-0.5));
#3444=CARTESIAN_POINT('',(0.288675134594813,0.,-0.5));
#3445=CARTESIAN_POINT('',(-0.288675134594813,0.,-0.5));
#3446=CARTESIAN_POINT('Origin',(0.577350269189626,0.,0.));
#3447=CARTESIAN_POINT('',(0.577350269189626,0.,0.));
#3448=CARTESIAN_POINT('',(0.577350269189626,0.,0.));
#3449=CARTESIAN_POINT('',(0.577350269189626,0.,0.));
#3450=CARTESIAN_POINT('Origin',(0.288675134594813,0.,0.5));
#3451=CARTESIAN_POINT('',(0.288675134594813,0.,0.5));
#3452=CARTESIAN_POINT('',(0.288675134594813,0.,0.5));
#3453=CARTESIAN_POINT('',(0.288675134594813,0.,0.5));
#3454=CARTESIAN_POINT('Origin',(-0.288675134594813,0.,0.5));
#3455=CARTESIAN_POINT('',(-0.288675134594813,0.,0.5));
#3456=CARTESIAN_POINT('',(-0.288675134594813,0.,0.5));
#3457=CARTESIAN_POINT('',(-0.288675134594813,0.,0.5));
#3458=CARTESIAN_POINT('Origin',(-0.577350269189626,0.,-7.07050159149938E-17));
#3459=CARTESIAN_POINT('',(-0.577350269189626,0.,-7.07050159149938E-17));
#3460=CARTESIAN_POINT('',(-0.577350269189626,0.,-7.07050159149938E-17));
#3461=CARTESIAN_POINT('',(-0.577350269189626,0.,-7.07050159149938E-17));
#3462=CARTESIAN_POINT('Origin',(-0.288675134594813,0.,-0.5));
#3463=CARTESIAN_POINT('',(-0.288675134594813,0.,-0.5));
#3464=CARTESIAN_POINT('Origin',(0.,0.4,0.));
#3465=CARTESIAN_POINT('Origin',(0.,0.,0.));
#3466=CARTESIAN_POINT('',(0.,0.,0.));
#3467=CARTESIAN_POINT('',(0.,0.,0.));
#3468=CARTESIAN_POINT('',(0.,0.,0.));
#3469=CARTESIAN_POINT('',(0.,0.,0.));
#3470=CARTESIAN_POINT('',(1.6,-1.8,28.));
#3471=CARTESIAN_POINT('',(0.,0.,0.));
#3472=CARTESIAN_POINT('',(0.,0.,0.));
#3473=CARTESIAN_POINT('Origin',(-0.1,0.82,-0.3));
#3474=CARTESIAN_POINT('',(0.,0.82,-0.3));
#3475=CARTESIAN_POINT('',(0.,1.,-0.3));
#3476=CARTESIAN_POINT('',(0.,0.41,-0.3));
#3477=CARTESIAN_POINT('',(30.,0.82,-0.3));
#3478=CARTESIAN_POINT('',(-0.1,0.82,-0.3));
#3479=CARTESIAN_POINT('',(30.,1.,-0.3));
#3480=CARTESIAN_POINT('',(30.,0.41,-0.3));
#3481=CARTESIAN_POINT('',(-0.05,1.,-0.3));
#3482=CARTESIAN_POINT('Origin',(-0.1,0.82,-0.55));
#3483=CARTESIAN_POINT('',(0.,0.82,-0.55));
#3484=CARTESIAN_POINT('',(0.,0.82,-0.275));
#3485=CARTESIAN_POINT('',(30.,0.82,-0.55));
#3486=CARTESIAN_POINT('',(-0.1,0.82,-0.55));
#3487=CARTESIAN_POINT('',(30.,0.82,-0.275));
#3488=CARTESIAN_POINT('Origin',(-0.1,0.67,-0.55));
#3489=CARTESIAN_POINT('',(0.,0.67,-0.55));
#3490=CARTESIAN_POINT('',(0.,0.335,-0.55));
#3491=CARTESIAN_POINT('',(30.,0.67,-0.55));
#3492=CARTESIAN_POINT('',(-0.1,0.67,-0.55));
#3493=CARTESIAN_POINT('',(30.,0.335,-0.55));
#3494=CARTESIAN_POINT('Origin',(-0.1,0.42,-0.3));
#3495=CARTESIAN_POINT('',(0.,0.42,-0.3));
#3496=CARTESIAN_POINT('',(0.,0.24,-0.12));
#3497=CARTESIAN_POINT('',(30.,0.42,-0.3));
#3498=CARTESIAN_POINT('',(-0.1,0.42,-0.3));
#3499=CARTESIAN_POINT('',(30.,0.24,-0.12));
#3500=CARTESIAN_POINT('Origin',(-0.1,0.42,0.3));
#3501=CARTESIAN_POINT('',(0.,0.42,0.3));
#3502=CARTESIAN_POINT('',(0.,0.42,0.15));
#3503=CARTESIAN_POINT('',(30.,0.42,0.3));
#3504=CARTESIAN_POINT('',(-0.1,0.42,0.3));
#3505=CARTESIAN_POINT('',(30.,0.42,0.15));
#3506=CARTESIAN_POINT('Origin',(-0.1,0.67,0.55));
#3507=CARTESIAN_POINT('',(0.,0.67,0.55));
#3508=CARTESIAN_POINT('',(6.93889390390723E-18,0.365,0.245));
#3509=CARTESIAN_POINT('',(30.,0.67,0.55));
#3510=CARTESIAN_POINT('',(-0.1,0.67,0.55));
#3511=CARTESIAN_POINT('',(30.,0.365,0.245));
#3512=CARTESIAN_POINT('Origin',(-0.1,0.82,0.55));
#3513=CARTESIAN_POINT('',(0.,0.82,0.55));
#3514=CARTESIAN_POINT('',(0.,0.41,0.55));
#3515=CARTESIAN_POINT('',(30.,0.82,0.55));
#3516=CARTESIAN_POINT('',(-0.1,0.82,0.55));
#3517=CARTESIAN_POINT('',(30.,0.41,0.55));
#3518=CARTESIAN_POINT('Origin',(-0.1,0.82,0.3));
#3519=CARTESIAN_POINT('',(0.,0.82,0.3));
#3520=CARTESIAN_POINT('',(0.,0.82,0.15));
#3521=CARTESIAN_POINT('',(30.,0.82,0.3));
#3522=CARTESIAN_POINT('',(-0.1,0.82,0.3));
#3523=CARTESIAN_POINT('',(30.,0.82,0.15));
#3524=CARTESIAN_POINT('Origin',(-0.1,1.05,0.3));
#3525=CARTESIAN_POINT('',(0.,1.,0.3));
#3526=CARTESIAN_POINT('',(0.,0.525,0.3));
#3527=CARTESIAN_POINT('',(30.,1.,0.3));
#3528=CARTESIAN_POINT('',(-0.05,1.,0.3));
#3529=CARTESIAN_POINT('',(30.,0.525,0.3));
#3530=CARTESIAN_POINT('Origin',(-0.1,-0.3,-0.82));
#3531=CARTESIAN_POINT('',(0.,-0.3,-0.82));
#3532=CARTESIAN_POINT('',(0.,-0.3,-1.));
#3533=CARTESIAN_POINT('',(0.,-0.3,-0.41));
#3534=CARTESIAN_POINT('',(30.,-0.3,-0.82));
#3535=CARTESIAN_POINT('',(-0.1,-0.3,-0.82));
#3536=CARTESIAN_POINT('',(30.,-0.3,-1.));
#3537=CARTESIAN_POINT('',(30.,-0.3,-0.41));
#3538=CARTESIAN_POINT('',(-0.05,-0.3,-1.));
#3539=CARTESIAN_POINT('Origin',(-0.1,-0.55,-0.82));
#3540=CARTESIAN_POINT('',(0.,-0.55,-0.82));
#3541=CARTESIAN_POINT('',(0.,-0.275,-0.82));
#3542=CARTESIAN_POINT('',(30.,-0.55,-0.82));
#3543=CARTESIAN_POINT('',(-0.1,-0.55,-0.82));
#3544=CARTESIAN_POINT('',(30.,-0.275,-0.82));
#3545=CARTESIAN_POINT('Origin',(-0.1,-0.55,-0.67));
#3546=CARTESIAN_POINT('',(0.,-0.55,-0.67));
#3547=CARTESIAN_POINT('',(0.,-0.55,-0.335));
#3548=CARTESIAN_POINT('',(30.,-0.55,-0.67));
#3549=CARTESIAN_POINT('',(-0.1,-0.55,-0.67));
#3550=CARTESIAN_POINT('',(30.,-0.55,-0.335));
#3551=CARTESIAN_POINT('Origin',(-0.1,-0.3,-0.42));
#3552=CARTESIAN_POINT('',(0.,-0.3,-0.42));
#3553=CARTESIAN_POINT('',(0.,-0.12,-0.24));
#3554=CARTESIAN_POINT('',(30.,-0.3,-0.42));
#3555=CARTESIAN_POINT('',(-0.1,-0.3,-0.42));
#3556=CARTESIAN_POINT('',(30.,-0.12,-0.24));
#3557=CARTESIAN_POINT('Origin',(-0.1,0.3,-0.42));
#3558=CARTESIAN_POINT('',(0.,0.3,-0.42));
#3559=CARTESIAN_POINT('',(0.,0.15,-0.42));
#3560=CARTESIAN_POINT('',(30.,0.3,-0.42));
#3561=CARTESIAN_POINT('',(-0.1,0.3,-0.42));
#3562=CARTESIAN_POINT('',(30.,0.15,-0.42));
#3563=CARTESIAN_POINT('Origin',(-0.1,0.55,-0.67));
#3564=CARTESIAN_POINT('',(0.,0.55,-0.67));
#3565=CARTESIAN_POINT('',(0.,0.245,-0.365));
#3566=CARTESIAN_POINT('',(30.,0.55,-0.67));
#3567=CARTESIAN_POINT('',(-0.1,0.55,-0.67));
#3568=CARTESIAN_POINT('',(30.,0.245,-0.365));
#3569=CARTESIAN_POINT('Origin',(-0.1,0.55,-0.82));
#3570=CARTESIAN_POINT('',(0.,0.55,-0.82));
#3571=CARTESIAN_POINT('',(0.,0.55,-0.41));
#3572=CARTESIAN_POINT('',(30.,0.55,-0.82));
#3573=CARTESIAN_POINT('',(-0.1,0.55,-0.82));
#3574=CARTESIAN_POINT('',(30.,0.55,-0.41));
#3575=CARTESIAN_POINT('Origin',(-0.1,0.3,-0.82));
#3576=CARTESIAN_POINT('',(0.,0.3,-0.82));
#3577=CARTESIAN_POINT('',(0.,0.15,-0.82));
#3578=CARTESIAN_POINT('',(30.,0.3,-0.82));
#3579=CARTESIAN_POINT('',(-0.1,0.3,-0.82));
#3580=CARTESIAN_POINT('',(30.,0.15,-0.82));
#3581=CARTESIAN_POINT('Origin',(-0.1,0.3,-1.05));
#3582=CARTESIAN_POINT('',(0.,0.3,-1.));
#3583=CARTESIAN_POINT('',(0.,0.3,-0.525));
#3584=CARTESIAN_POINT('',(30.,0.3,-1.));
#3585=CARTESIAN_POINT('',(-0.05,0.3,-1.));
#3586=CARTESIAN_POINT('',(30.,0.3,-0.525));
#3587=CARTESIAN_POINT('Origin',(-0.1,-0.82,0.3));
#3588=CARTESIAN_POINT('',(0.,-0.82,0.3));
#3589=CARTESIAN_POINT('',(0.,-1.,0.3));
#3590=CARTESIAN_POINT('',(0.,-0.41,0.3));
#3591=CARTESIAN_POINT('',(30.,-0.82,0.3));
#3592=CARTESIAN_POINT('',(-0.1,-0.82,0.3));
#3593=CARTESIAN_POINT('',(30.,-1.,0.3));
#3594=CARTESIAN_POINT('',(30.,-0.41,0.3));
#3595=CARTESIAN_POINT('',(-0.05,-1.,0.3));
#3596=CARTESIAN_POINT('Origin',(-0.1,-0.82,0.55));
#3597=CARTESIAN_POINT('',(0.,-0.82,0.55));
#3598=CARTESIAN_POINT('',(0.,-0.82,0.275));
#3599=CARTESIAN_POINT('',(30.,-0.82,0.55));
#3600=CARTESIAN_POINT('',(-0.1,-0.82,0.55));
#3601=CARTESIAN_POINT('',(30.,-0.82,0.275));
#3602=CARTESIAN_POINT('Origin',(-0.1,-0.67,0.55));
#3603=CARTESIAN_POINT('',(0.,-0.67,0.55));
#3604=CARTESIAN_POINT('',(0.,-0.335,0.55));
#3605=CARTESIAN_POINT('',(30.,-0.67,0.55));
#3606=CARTESIAN_POINT('',(-0.1,-0.67,0.55));
#3607=CARTESIAN_POINT('',(30.,-0.335,0.55));
#3608=CARTESIAN_POINT('Origin',(-0.1,-0.42,0.3));
#3609=CARTESIAN_POINT('',(0.,-0.42,0.3));
#3610=CARTESIAN_POINT('',(-6.93889390390723E-18,-0.24,0.12));
#3611=CARTESIAN_POINT('',(30.,-0.42,0.3));
#3612=CARTESIAN_POINT('',(-0.1,-0.42,0.3));
#3613=CARTESIAN_POINT('',(30.,-0.24,0.12));
#3614=CARTESIAN_POINT('Origin',(-0.1,-0.42,-0.3));
#3615=CARTESIAN_POINT('',(0.,-0.42,-0.3));
#3616=CARTESIAN_POINT('',(0.,-0.42,-0.15));
#3617=CARTESIAN_POINT('',(30.,-0.42,-0.3));
#3618=CARTESIAN_POINT('',(-0.1,-0.42,-0.3));
#3619=CARTESIAN_POINT('',(30.,-0.42,-0.15));
#3620=CARTESIAN_POINT('Origin',(-0.1,-0.67,-0.55));
#3621=CARTESIAN_POINT('',(0.,-0.67,-0.55));
#3622=CARTESIAN_POINT('',(0.,-0.365,-0.245));
#3623=CARTESIAN_POINT('',(30.,-0.67,-0.55));
#3624=CARTESIAN_POINT('',(-0.1,-0.67,-0.55));
#3625=CARTESIAN_POINT('',(30.,-0.365,-0.245));
#3626=CARTESIAN_POINT('Origin',(-0.1,-0.82,-0.55));
#3627=CARTESIAN_POINT('',(0.,-0.82,-0.55));
#3628=CARTESIAN_POINT('',(0.,-0.41,-0.55));
#3629=CARTESIAN_POINT('',(30.,-0.82,-0.55));
#3630=CARTESIAN_POINT('',(-0.1,-0.82,-0.55));
#3631=CARTESIAN_POINT('',(30.,-0.41,-0.55));
#3632=CARTESIAN_POINT('Origin',(-0.1,-0.82,-0.3));
#3633=CARTESIAN_POINT('',(0.,-0.82,-0.3));
#3634=CARTESIAN_POINT('',(0.,-0.82,-0.15));
#3635=CARTESIAN_POINT('',(30.,-0.82,-0.3));
#3636=CARTESIAN_POINT('',(-0.1,-0.82,-0.3));
#3637=CARTESIAN_POINT('',(30.,-0.82,-0.15));
#3638=CARTESIAN_POINT('Origin',(-0.1,-1.05,-0.3));
#3639=CARTESIAN_POINT('',(0.,-1.,-0.3));
#3640=CARTESIAN_POINT('',(0.,-0.525,-0.3));
#3641=CARTESIAN_POINT('',(30.,-1.,-0.3));
#3642=CARTESIAN_POINT('',(-0.05,-1.,-0.3));
#3643=CARTESIAN_POINT('',(30.,-0.525,-0.3));
#3644=CARTESIAN_POINT('Origin',(-0.1,0.3,0.82));
#3645=CARTESIAN_POINT('',(0.,0.3,0.82));
#3646=CARTESIAN_POINT('',(0.,0.3,1.));
#3647=CARTESIAN_POINT('',(0.,0.3,0.41));
#3648=CARTESIAN_POINT('',(30.,0.3,0.82));
#3649=CARTESIAN_POINT('',(-0.1,0.3,0.82));
#3650=CARTESIAN_POINT('',(30.,0.3,1.));
#3651=CARTESIAN_POINT('',(30.,0.3,0.41));
#3652=CARTESIAN_POINT('',(-0.05,0.3,1.));
#3653=CARTESIAN_POINT('Origin',(-0.1,0.55,0.82));
#3654=CARTESIAN_POINT('',(0.,0.55,0.82));
#3655=CARTESIAN_POINT('',(0.,0.275,0.82));
#3656=CARTESIAN_POINT('',(30.,0.55,0.82));
#3657=CARTESIAN_POINT('',(-0.1,0.55,0.82));
#3658=CARTESIAN_POINT('',(30.,0.275,0.82));
#3659=CARTESIAN_POINT('Origin',(-0.1,0.55,0.67));
#3660=CARTESIAN_POINT('',(0.,0.55,0.67));
#3661=CARTESIAN_POINT('',(0.,0.55,0.335));
#3662=CARTESIAN_POINT('',(30.,0.55,0.67));
#3663=CARTESIAN_POINT('',(-0.1,0.55,0.67));
#3664=CARTESIAN_POINT('',(30.,0.55,0.335));
#3665=CARTESIAN_POINT('Origin',(-0.1,0.3,0.42));
#3666=CARTESIAN_POINT('',(0.,0.3,0.42));
#3667=CARTESIAN_POINT('',(6.93889390390723E-18,0.12,0.24));
#3668=CARTESIAN_POINT('',(30.,0.3,0.42));
#3669=CARTESIAN_POINT('',(-0.1,0.3,0.42));
#3670=CARTESIAN_POINT('',(30.,0.12,0.24));
#3671=CARTESIAN_POINT('Origin',(-0.1,-0.3,0.42));
#3672=CARTESIAN_POINT('',(0.,-0.3,0.42));
#3673=CARTESIAN_POINT('',(0.,-0.15,0.42));
#3674=CARTESIAN_POINT('',(30.,-0.3,0.42));
#3675=CARTESIAN_POINT('',(-0.1,-0.3,0.42));
#3676=CARTESIAN_POINT('',(30.,-0.15,0.42));
#3677=CARTESIAN_POINT('Origin',(-0.1,-0.55,0.67));
#3678=CARTESIAN_POINT('',(0.,-0.55,0.67));
#3679=CARTESIAN_POINT('',(6.93889390390723E-18,-0.245,0.365));
#3680=CARTESIAN_POINT('',(30.,-0.55,0.67));
#3681=CARTESIAN_POINT('',(-0.1,-0.55,0.67));
#3682=CARTESIAN_POINT('',(30.,-0.245,0.365));
#3683=CARTESIAN_POINT('Origin',(-0.1,-0.55,0.82));
#3684=CARTESIAN_POINT('',(0.,-0.55,0.82));
#3685=CARTESIAN_POINT('',(0.,-0.55,0.41));
#3686=CARTESIAN_POINT('',(30.,-0.55,0.82));
#3687=CARTESIAN_POINT('',(-0.1,-0.55,0.82));
#3688=CARTESIAN_POINT('',(30.,-0.55,0.41));
#3689=CARTESIAN_POINT('Origin',(-0.1,-0.3,0.82));
#3690=CARTESIAN_POINT('',(0.,-0.3,0.82));
#3691=CARTESIAN_POINT('',(0.,-0.15,0.82));
#3692=CARTESIAN_POINT('',(30.,-0.3,0.82));
#3693=CARTESIAN_POINT('',(-0.1,-0.3,0.82));
#3694=CARTESIAN_POINT('',(30.,-0.15,0.82));
#3695=CARTESIAN_POINT('Origin',(-0.1,-0.3,1.05));
#3696=CARTESIAN_POINT('',(0.,-0.3,1.));
#3697=CARTESIAN_POINT('',(0.,-0.3,0.525));
#3698=CARTESIAN_POINT('',(30.,-0.3,1.));
#3699=CARTESIAN_POINT('',(-0.05,-0.3,1.));
#3700=CARTESIAN_POINT('',(30.,-0.3,0.525));
#3701=CARTESIAN_POINT('Origin',(-0.1,0.,0.));
#3702=CARTESIAN_POINT('',(0.,-2.57175827820944E-17,0.21));
#3703=CARTESIAN_POINT('Origin',(0.,0.,0.));
#3704=CARTESIAN_POINT('',(30.,2.57175827820944E-17,0.21));
#3705=CARTESIAN_POINT('',(-0.1,-2.57175827820944E-17,0.21));
#3706=CARTESIAN_POINT('Origin',(30.,0.,0.));
#3707=CARTESIAN_POINT('Origin',(0.,1.,-1.));
#3708=CARTESIAN_POINT('',(0.,1.,1.));
#3709=CARTESIAN_POINT('',(0.,1.,-1.));
#3710=CARTESIAN_POINT('',(30.,1.,1.));
#3711=CARTESIAN_POINT('',(0.,1.,1.));
#3712=CARTESIAN_POINT('',(30.,1.,-1.));
#3713=CARTESIAN_POINT('Origin',(0.,1.,-1.));
#3714=CARTESIAN_POINT('',(30.,1.,-1.));
#3715=CARTESIAN_POINT('',(30.,1.,-1.));
#3716=CARTESIAN_POINT('',(0.,1.,-1.));
#3717=CARTESIAN_POINT('',(0.,1.,-1.));
#3718=CARTESIAN_POINT('',(0.,1.,-1.));
#3719=CARTESIAN_POINT('Origin',(0.,-1.,-1.));
#3720=CARTESIAN_POINT('',(0.,-1.,-1.));
#3721=CARTESIAN_POINT('',(30.,-1.,-1.));
#3722=CARTESIAN_POINT('Origin',(0.,-1.,-1.));
#3723=CARTESIAN_POINT('',(30.,-1.,-1.));
#3724=CARTESIAN_POINT('',(30.,-1.,-1.));
#3725=CARTESIAN_POINT('',(0.,-1.,-1.));
#3726=CARTESIAN_POINT('',(0.,-1.,-1.));
#3727=CARTESIAN_POINT('',(0.,-1.,-1.));
#3728=CARTESIAN_POINT('Origin',(0.,-1.,1.));
#3729=CARTESIAN_POINT('',(0.,-1.,1.));
#3730=CARTESIAN_POINT('',(30.,-1.,1.));
#3731=CARTESIAN_POINT('Origin',(0.,-1.,1.));
#3732=CARTESIAN_POINT('',(30.,-1.,1.));
#3733=CARTESIAN_POINT('',(30.,-1.,1.));
#3734=CARTESIAN_POINT('',(0.,-1.,1.));
#3735=CARTESIAN_POINT('',(0.,-1.,1.));
#3736=CARTESIAN_POINT('',(0.,-1.,1.));
#3737=CARTESIAN_POINT('Origin',(0.,1.,1.));
#3738=CARTESIAN_POINT('',(0.,1.,1.));
#3739=CARTESIAN_POINT('',(30.,1.,1.));
#3740=CARTESIAN_POINT('Origin',(0.,1.,1.));
#3741=CARTESIAN_POINT('',(30.,1.,1.));
#3742=CARTESIAN_POINT('',(0.,1.,1.));
#3743=CARTESIAN_POINT('Origin',(30.,0.,0.));
#3744=CARTESIAN_POINT('Origin',(0.,0.,0.));
#3745=CARTESIAN_POINT('',(0.,0.,12.));
#3746=CARTESIAN_POINT('',(0.,0.,0.));
#3747=CARTESIAN_POINT('',(0.,0.,0.));
#3748=UNCERTAINTY_MEASURE_WITH_UNIT(LENGTH_MEASURE(0.001),#3774,
'DISTANCE_ACCURACY_VALUE',
'Maximum model space distance between geometric entities at asserted c
onnectivities');
#3749=UNCERTAINTY_MEASURE_WITH_UNIT(LENGTH_MEASURE(0.001),#3774,
'DISTANCE_ACCURACY_VALUE',
'Maximum model space distance between geometric entities at asserted c
onnectivities');
#3750=UNCERTAINTY_MEASURE_WITH_UNIT(LENGTH_MEASURE(0.001),#3774,
'DISTANCE_ACCURACY_VALUE',
'Maximum model space distance between geometric entities at asserted c
onnectivities');
#3751=UNCERTAINTY_MEASURE_WITH_UNIT(LENGTH_MEASURE(0.001),#3774,
'DISTANCE_ACCURACY_VALUE',
'Maximum model space distance between geometric entities at asserted c
onnectivities');
#3752=UNCERTAINTY_MEASURE_WITH_UNIT(LENGTH_MEASURE(0.001),#3774,
'DISTANCE_ACCURACY_VALUE',
'Maximum model space distance between geometric entities at asserted c
onnectivities');
#3753=UNCERTAINTY_MEASURE_WITH_UNIT(LENGTH_MEASURE(0.001),#3774,
'DISTANCE_ACCURACY_VALUE',
'Maximum model space distance between geometric entities at asserted c
onnectivities');
#3754=UNCERTAINTY_MEASURE_WITH_UNIT(LENGTH_MEASURE(0.001),#3774,
'DISTANCE_ACCURACY_VALUE',
'Maximum model space distance between geometric entities at asserted c
onnectivities');
#3755=UNCERTAINTY_MEASURE_WITH_UNIT(LENGTH_MEASURE(0.001),#3774,
'DISTANCE_ACCURACY_VALUE',
'Maximum model space distance between geometric entities at asserted c
onnectivities');
#3756=UNCERTAINTY_MEASURE_WITH_UNIT(LENGTH_MEASURE(0.001),#3774,
'DISTANCE_ACCURACY_VALUE',
'Maximum model space distance between geometric entities at asserted c
onnectivities');
#3757=UNCERTAINTY_MEASURE_WITH_UNIT(LENGTH_MEASURE(0.001),#3774,
'DISTANCE_ACCURACY_VALUE',
'Maximum model space distance between geometric entities at asserted c
onnectivities');
#3758=UNCERTAINTY_MEASURE_WITH_UNIT(LENGTH_MEASURE(0.001),#3774,
'DISTANCE_ACCURACY_VALUE',
'Maximum model space distance between geometric entities at asserted c
onnectivities');
#3759=UNCERTAINTY_MEASURE_WITH_UNIT(LENGTH_MEASURE(0.001),#3774,
'DISTANCE_ACCURACY_VALUE',
'Maximum model space distance between geometric entities at asserted c
onnectivities');
#3760=UNCERTAINTY_MEASURE_WITH_UNIT(LENGTH_MEASURE(0.001),#3774,
'DISTANCE_ACCURACY_VALUE',
'Maximum model space distance between geometric entities at asserted c
onnectivities');
#3761=(
GEOMETRIC_REPRESENTATION_CONTEXT(3)
GLOBAL_UNCERTAINTY_ASSIGNED_CONTEXT((#3748))
GLOBAL_UNIT_ASSIGNED_CONTEXT((#3774,#3776,#3777))
REPRESENTATION_CONTEXT('','3D')
);
#3762=(
GEOMETRIC_REPRESENTATION_CONTEXT(3)
GLOBAL_UNCERTAINTY_ASSIGNED_CONTEXT((#3749))
GLOBAL_UNIT_ASSIGNED_CONTEXT((#3774,#3776,#3777))
REPRESENTATION_CONTEXT('','3D')
);
#3763=(
GEOMETRIC_REPRESENTATION_CONTEXT(3)
GLOBAL_UNCERTAINTY_ASSIGNED_CONTEXT((#3750))
GLOBAL_UNIT_ASSIGNED_CONTEXT((#3774,#3776,#3777))
REPRESENTATION_CONTEXT('','3D')
);
#3764=(
GEOMETRIC_REPRESENTATION_CONTEXT(3)
GLOBAL_UNCERTAINTY_ASSIGNED_CONTEXT((#3751))
GLOBAL_UNIT_ASSIGNED_CONTEXT((#3774,#3776,#3777))
REPRESENTATION_CONTEXT('','3D')
);
#3765=(
GEOMETRIC_REPRESENTATION_CONTEXT(3)
GLOBAL_UNCERTAINTY_ASSIGNED_CONTEXT((#3752))
GLOBAL_UNIT_ASSIGNED_CONTEXT((#3774,#3776,#3777))
REPRESENTATION_CONTEXT('','3D')
);
#3766=(
GEOMETRIC_REPRESENTATION_CONTEXT(3)
GLOBAL_UNCERTAINTY_ASSIGNED_CONTEXT((#3753))
GLOBAL_UNIT_ASSIGNED_CONTEXT((#3774,#3776,#3777))
REPRESENTATION_CONTEXT('','3D')
);
#3767=(
GEOMETRIC_REPRESENTATION_CONTEXT(3)
GLOBAL_UNCERTAINTY_ASSIGNED_CONTEXT((#3754))
GLOBAL_UNIT_ASSIGNED_CONTEXT((#3774,#3776,#3777))
REPRESENTATION_CONTEXT('','3D')
);
#3768=(
GEOMETRIC_REPRESENTATION_CONTEXT(3)
GLOBAL_UNCERTAINTY_ASSIGNED_CONTEXT((#3755))
GLOBAL_UNIT_ASSIGNED_CONTEXT((#3774,#3776,#3777))
REPRESENTATION_CONTEXT('','3D')
);
#3769=(
GEOMETRIC_REPRESENTATION_CONTEXT(3)
GLOBAL_UNCERTAINTY_ASSIGNED_CONTEXT((#3756))
GLOBAL_UNIT_ASSIGNED_CONTEXT((#3774,#3776,#3777))
REPRESENTATION_CONTEXT('','3D')
);
#3770=(
GEOMETRIC_REPRESENTATION_CONTEXT(3)
GLOBAL_UNCERTAINTY_ASSIGNED_CONTEXT((#3757))
GLOBAL_UNIT_ASSIGNED_CONTEXT((#3774,#3776,#3777))
REPRESENTATION_CONTEXT('','3D')
);
#3771=(
GEOMETRIC_REPRESENTATION_CONTEXT(3)
GLOBAL_UNCERTAINTY_ASSIGNED_CONTEXT((#3758))
GLOBAL_UNIT_ASSIGNED_CONTEXT((#3774,#3776,#3777))
REPRESENTATION_CONTEXT('','3D')
);
#3772=(
GEOMETRIC_REPRESENTATION_CONTEXT(3)
GLOBAL_UNCERTAINTY_ASSIGNED_CONTEXT((#3759))
GLOBAL_UNIT_ASSIGNED_CONTEXT((#3774,#3776,#3777))
REPRESENTATION_CONTEXT('','3D')
);
#3773=(
GEOMETRIC_REPRESENTATION_CONTEXT(3)
GLOBAL_UNCERTAINTY_ASSIGNED_CONTEXT((#3760))
GLOBAL_UNIT_ASSIGNED_CONTEXT((#3774,#3776,#3777))
REPRESENTATION_CONTEXT('','3D')
);
#3774=(
LENGTH_UNIT()
NAMED_UNIT(*)
SI_UNIT(.CENTI.,.METRE.)
);
#3775=(
LENGTH_UNIT()
NAMED_UNIT(*)
SI_UNIT($,.METRE.)
);
#3776=(
NAMED_UNIT(*)
PLANE_ANGLE_UNIT()
SI_UNIT($,.RADIAN.)
);
#3777=(
NAMED_UNIT(*)
SI_UNIT($,.STERADIAN.)
SOLID_ANGLE_UNIT()
);
#3778=SHAPE_DEFINITION_REPRESENTATION(#3790,#3813);
#3779=SHAPE_DEFINITION_REPRESENTATION(#3791,#3814);
#3780=SHAPE_DEFINITION_REPRESENTATION(#3792,#3815);
#3781=SHAPE_DEFINITION_REPRESENTATION(#3793,#3816);
#3782=SHAPE_DEFINITION_REPRESENTATION(#3794,#3817);
#3783=SHAPE_DEFINITION_REPRESENTATION(#3795,#3818);
#3784=SHAPE_DEFINITION_REPRESENTATION(#3796,#3819);
#3785=SHAPE_DEFINITION_REPRESENTATION(#3797,#3820);
#3786=SHAPE_DEFINITION_REPRESENTATION(#3798,#3821);
#3787=SHAPE_DEFINITION_REPRESENTATION(#3802,#3822);
#3788=SHAPE_DEFINITION_REPRESENTATION(#3808,#3823);
#3789=SHAPE_DEFINITION_REPRESENTATION(#3809,#3824);
#3790=PRODUCT_DEFINITION_SHAPE('',$,#3826);
#3791=PRODUCT_DEFINITION_SHAPE('',$,#3827);
#3792=PRODUCT_DEFINITION_SHAPE('',$,#3828);
#3793=PRODUCT_DEFINITION_SHAPE('',$,#3829);
#3794=PRODUCT_DEFINITION_SHAPE('',$,#3830);
#3795=PRODUCT_DEFINITION_SHAPE('',$,#3831);
#3796=PRODUCT_DEFINITION_SHAPE('',$,#3832);
#3797=PRODUCT_DEFINITION_SHAPE('',$,#3833);
#3798=PRODUCT_DEFINITION_SHAPE('',$,#3834);
#3799=PRODUCT_DEFINITION_SHAPE($,$,#50);
#3800=PRODUCT_DEFINITION_SHAPE($,$,#51);
#3801=PRODUCT_DEFINITION_SHAPE($,$,#52);
#3802=PRODUCT_DEFINITION_SHAPE('',$,#3835);
#3803=PRODUCT_DEFINITION_SHAPE($,$,#53);
#3804=PRODUCT_DEFINITION_SHAPE($,$,#54);
#3805=PRODUCT_DEFINITION_SHAPE($,$,#55);
#3806=PRODUCT_DEFINITION_SHAPE($,$,#56);
#3807=PRODUCT_DEFINITION_SHAPE($,$,#57);
#3808=PRODUCT_DEFINITION_SHAPE('',$,#3836);
#3809=PRODUCT_DEFINITION_SHAPE('',$,#3837);
#3810=PRODUCT_DEFINITION_SHAPE($,$,#58);
#3811=PRODUCT_DEFINITION_SHAPE($,$,#59);
#3812=PRODUCT_DEFINITION_SHAPE($,$,#60);
#3813=SHAPE_REPRESENTATION('',(#2334,#2500,#2501),#3761);
#3814=SHAPE_REPRESENTATION('',(#2335,#2443,#2444,#2445,#2446,#2447),#3762);
#3815=SHAPE_REPRESENTATION('',(#2336),#3763);
#3816=SHAPE_REPRESENTATION('',(#2346),#3764);
#3817=SHAPE_REPRESENTATION('',(#2357),#3765);
#3818=SHAPE_REPRESENTATION('',(#2383,#2423,#2424,#2425),#3766);
#3819=SHAPE_REPRESENTATION('',(#2384),#3767);
#3820=SHAPE_REPRESENTATION('',(#2392),#3768);
#3821=SHAPE_REPRESENTATION('',(#2403),#3769);
#3822=SHAPE_REPRESENTATION('',(#2426),#3770);
#3823=SHAPE_REPRESENTATION('',(#2448,#2499),#3771);
#3824=SHAPE_REPRESENTATION('',(#2449),#3772);
#3825=PRODUCT_DEFINITION_CONTEXT('part definition',#3863,'design');
#3826=PRODUCT_DEFINITION('PAT-023',
'PAT-023',#3838,#3825);
#3827=PRODUCT_DEFINITION('Foot and clamp assembly',
'Foot and clamp assembly',#3839,#3825);
#3828=PRODUCT_DEFINITION('Foot adapter','Foot adapter',#3840,
#3825);
#3829=PRODUCT_DEFINITION('Outer square sleeve',
'Outer square sleeve',#3841,#3825);
#3830=PRODUCT_DEFINITION('Split clamp block','Split clamp block',
#3842,#3825);
#3831=PRODUCT_DEFINITION('Levelling Foot - 40 mm Pad, M8 Stud',
'Levelling Foot - 40 mm Pad, M8 Stud',#3843,#3825);
#3832=PRODUCT_DEFINITION('Rubber base','Rubber base',#3844,
#3825);
#3833=PRODUCT_DEFINITION('Steel pad','Steel pad',#3845,#3825);
#3834=PRODUCT_DEFINITION('Stud','Stud',#3846,#3825);
#3835=PRODUCT_DEFINITION('Hex Bolt - M6 x 30 mm',
'Hex Bolt - M6 x 30 mm',#3847,#3825);
#3836=PRODUCT_DEFINITION('Sliding extrusion','Sliding extrusion',
#3848,#3825);
#3837=PRODUCT_DEFINITION('Slotted Extrusion - 20 x 20 x 300 mm',
'Slotted Extrusion - 20 x 20 x 300 mm',#3849,#3825);
#3838=PRODUCT_DEFINITION_FORMATION('',$,#3865);
#3839=PRODUCT_DEFINITION_FORMATION('',$,#3866);
#3840=PRODUCT_DEFINITION_FORMATION('',$,#3867);
#3841=PRODUCT_DEFINITION_FORMATION('',$,#3868);
#3842=PRODUCT_DEFINITION_FORMATION('',$,#3869);
#3843=PRODUCT_DEFINITION_FORMATION('',$,#3870);
#3844=PRODUCT_DEFINITION_FORMATION('',$,#3871);
#3845=PRODUCT_DEFINITION_FORMATION('',$,#3872);
#3846=PRODUCT_DEFINITION_FORMATION('',$,#3873);
#3847=PRODUCT_DEFINITION_FORMATION('',$,#3874);
#3848=PRODUCT_DEFINITION_FORMATION('',$,#3875);
#3849=PRODUCT_DEFINITION_FORMATION('',$,#3876);
#3850=PRODUCT_RELATED_PRODUCT_CATEGORY('PAT-023',
'PAT-023',(#3865));
#3851=PRODUCT_RELATED_PRODUCT_CATEGORY('Foot and clamp assembly',
'Foot and clamp assembly',(#3866));
#3852=PRODUCT_RELATED_PRODUCT_CATEGORY('Foot adapter','Foot adapter',(#3867));
#3853=PRODUCT_RELATED_PRODUCT_CATEGORY('Outer square sleeve',
'Outer square sleeve',(#3868));
#3854=PRODUCT_RELATED_PRODUCT_CATEGORY('Split clamp block',
'Split clamp block',(#3869));
#3855=PRODUCT_RELATED_PRODUCT_CATEGORY(
'Levelling Foot - 40 mm Pad, M8 Stud',
'Levelling Foot - 40 mm Pad, M8 Stud',(#3870));
#3856=PRODUCT_RELATED_PRODUCT_CATEGORY('Rubber base','Rubber base',(#3871));
#3857=PRODUCT_RELATED_PRODUCT_CATEGORY('Steel pad','Steel pad',(#3872));
#3858=PRODUCT_RELATED_PRODUCT_CATEGORY('Stud','Stud',(#3873));
#3859=PRODUCT_RELATED_PRODUCT_CATEGORY('Hex Bolt - M6 x 30 mm',
'Hex Bolt - M6 x 30 mm',(#3874));
#3860=PRODUCT_RELATED_PRODUCT_CATEGORY('Sliding extrusion',
'Sliding extrusion',(#3875));
#3861=PRODUCT_RELATED_PRODUCT_CATEGORY(
'Slotted Extrusion - 20 x 20 x 300 mm',
'Slotted Extrusion - 20 x 20 x 300 mm',(#3876));
#3862=APPLICATION_PROTOCOL_DEFINITION('international standard',
'automotive_design',2009,#3863);
#3863=APPLICATION_CONTEXT(
'Core Data for Automotive Mechanical Design Process');
#3864=PRODUCT_CONTEXT('part definition',#3863,'mechanical');
#3865=PRODUCT('PAT-023','PAT-023',
'PAT-023',(#3864));
#3866=PRODUCT('Foot and clamp assembly','Foot and clamp assembly',
'Foot and clamp assembly',(#3864));
#3867=PRODUCT('Foot adapter','Foot adapter','Foot adapter',(#3864));
#3868=PRODUCT('Outer square sleeve','Outer square sleeve',
'Outer square sleeve',(#3864));
#3869=PRODUCT('Split clamp block','Split clamp block',
'Split clamp block',(#3864));
#3870=PRODUCT('Levelling Foot - 40 mm Pad, M8 Stud',
'Levelling Foot - 40 mm Pad, M8 Stud',
'Levelling Foot - 40 mm Pad, M8 Stud',(#3864));
#3871=PRODUCT('Rubber base','Rubber base','Rubber base',(#3864));
#3872=PRODUCT('Steel pad','Steel pad','Steel pad',(#3864));
#3873=PRODUCT('Stud','Stud','Stud',(#3864));
#3874=PRODUCT('Hex Bolt - M6 x 30 mm','Hex Bolt - M6 x 30 mm',
'Hex Bolt - M6 x 30 mm',(#3864));
#3875=PRODUCT('Sliding extrusion','Sliding extrusion',
'Sliding extrusion',(#3864));
#3876=PRODUCT('Slotted Extrusion - 20 x 20 x 300 mm',
'Slotted Extrusion - 20 x 20 x 300 mm',
'Slotted Extrusion - 20 x 20 x 300 mm',(#3864));
#3877=PRESENTATION_STYLE_ASSIGNMENT((#3883));
#3878=PRESENTATION_STYLE_ASSIGNMENT((#3884));
#3879=PRESENTATION_STYLE_ASSIGNMENT((#3885));
#3880=PRESENTATION_STYLE_ASSIGNMENT((#3886));
#3881=PRESENTATION_STYLE_ASSIGNMENT((#3887));
#3882=PRESENTATION_STYLE_ASSIGNMENT((#3888));
#3883=SURFACE_STYLE_USAGE(.BOTH.,#3889);
#3884=SURFACE_STYLE_USAGE(.BOTH.,#3890);
#3885=SURFACE_STYLE_USAGE(.BOTH.,#3891);
#3886=SURFACE_STYLE_USAGE(.BOTH.,#3892);
#3887=SURFACE_STYLE_USAGE(.BOTH.,#3893);
#3888=SURFACE_STYLE_USAGE(.BOTH.,#3894);
#3889=SURFACE_SIDE_STYLE('',(#3895));
#3890=SURFACE_SIDE_STYLE('',(#3896));
#3891=SURFACE_SIDE_STYLE('',(#3897));
#3892=SURFACE_SIDE_STYLE('',(#3898));
#3893=SURFACE_SIDE_STYLE('',(#3899));
#3894=SURFACE_SIDE_STYLE('',(#3900));
#3895=SURFACE_STYLE_FILL_AREA(#3901);
#3896=SURFACE_STYLE_FILL_AREA(#3902);
#3897=SURFACE_STYLE_FILL_AREA(#3903);
#3898=SURFACE_STYLE_FILL_AREA(#3904);
#3899=SURFACE_STYLE_FILL_AREA(#3905);
#3900=SURFACE_STYLE_FILL_AREA(#3906);
#3901=FILL_AREA_STYLE('Steel - Satin',(#3907));
#3902=FILL_AREA_STYLE('CAD Library Painted - Deep blue',(#3908));
#3903=FILL_AREA_STYLE('CAD Library Painted - Steel gray',(#3909));
#3904=FILL_AREA_STYLE('CAD Library Painted - Light blue',(#3910));
#3905=FILL_AREA_STYLE('CAD Library Painted - Graphite',(#3911));
#3906=FILL_AREA_STYLE('CAD Library Painted - Off white',(#3912));
#3907=FILL_AREA_STYLE_COLOUR('Steel - Satin',#3913);
#3908=FILL_AREA_STYLE_COLOUR('CAD Library Painted - Deep blue',#3914);
#3909=FILL_AREA_STYLE_COLOUR('CAD Library Painted - Steel gray',#3915);
#3910=FILL_AREA_STYLE_COLOUR('CAD Library Painted - Light blue',#3916);
#3911=FILL_AREA_STYLE_COLOUR('CAD Library Painted - Graphite',#3917);
#3912=FILL_AREA_STYLE_COLOUR('CAD Library Painted - Off white',#3918);
#3913=COLOUR_RGB('Steel - Satin',0.627450980392157,0.627450980392157,0.627450980392157);
#3914=COLOUR_RGB('CAD Library Painted - Deep blue',0.0784313725490196,0.203921568627451,
0.349019607843137);
#3915=COLOUR_RGB('CAD Library Painted - Steel gray',0.592156862745098,0.631372549019608,
0.67843137254902);
#3916=COLOUR_RGB('CAD Library Painted - Light blue',0.286274509803922,0.552941176470588,
0.780392156862745);
#3917=COLOUR_RGB('CAD Library Painted - Graphite',0.0980392156862745,0.109803921568627,
0.125490196078431);
#3918=COLOUR_RGB('CAD Library Painted - Off white',0.909803921568627,0.901960784313726,
0.858823529411765);
#3919=COLOUR_RGB('Dark Blue',0.08,0.2,0.34);
#3920=FILL_AREA_STYLE_COLOUR('',#3919);
#3921=FILL_AREA_STYLE('',(#3920));
#3922=SURFACE_STYLE_FILL_AREA(#3921);
#3923=SURFACE_SIDE_STYLE('',(#3922));
#3924=SURFACE_STYLE_USAGE(.BOTH.,#3923);
#3925=PRESENTATION_STYLE_ASSIGNMENT((#3924));
#3926=COLOUR_RGB('Light Blue',0.38,0.62,0.78);
#3927=FILL_AREA_STYLE_COLOUR('',#3926);
#3928=FILL_AREA_STYLE('',(#3927));
#3929=SURFACE_STYLE_FILL_AREA(#3928);
#3930=SURFACE_SIDE_STYLE('',(#3929));
#3931=SURFACE_STYLE_USAGE(.BOTH.,#3930);
#3932=PRESENTATION_STYLE_ASSIGNMENT((#3931));
#3933=COLOUR_RGB('Sky Blue',0.24,0.69,0.87);
#3934=FILL_AREA_STYLE_COLOUR('',#3933);
#3935=FILL_AREA_STYLE('',(#3934));
#3936=SURFACE_STYLE_FILL_AREA(#3935);
#3937=SURFACE_SIDE_STYLE('',(#3936));
#3938=SURFACE_STYLE_USAGE(.BOTH.,#3937);
#3939=PRESENTATION_STYLE_ASSIGNMENT((#3938));
#3940=COLOUR_RGB('Grey',0.48,0.52,0.57);
#3941=FILL_AREA_STYLE_COLOUR('',#3940);
#3942=FILL_AREA_STYLE('',(#3941));
#3943=SURFACE_STYLE_FILL_AREA(#3942);
#3944=SURFACE_SIDE_STYLE('',(#3943));
#3945=SURFACE_STYLE_USAGE(.BOTH.,#3944);
#3946=PRESENTATION_STYLE_ASSIGNMENT((#3945));
#3947=COLOUR_RGB('Black',0.12,0.14,0.17);
#3948=FILL_AREA_STYLE_COLOUR('',#3947);
#3949=FILL_AREA_STYLE('',(#3948));
#3950=SURFACE_STYLE_FILL_AREA(#3949);
#3951=SURFACE_SIDE_STYLE('',(#3950));
#3952=SURFACE_STYLE_USAGE(.BOTH.,#3951);
#3953=PRESENTATION_STYLE_ASSIGNMENT((#3952));
#3954=COLOUR_RGB('Off White',0.89,0.88,0.83);
#3955=FILL_AREA_STYLE_COLOUR('',#3954);
#3956=FILL_AREA_STYLE('',(#3955));
#3957=SURFACE_STYLE_FILL_AREA(#3956);
#3958=SURFACE_SIDE_STYLE('',(#3957));
#3959=SURFACE_STYLE_USAGE(.BOTH.,#3958);
#3960=PRESENTATION_STYLE_ASSIGNMENT((#3959));
ENDSEC;
END-ISO-10303-21;
